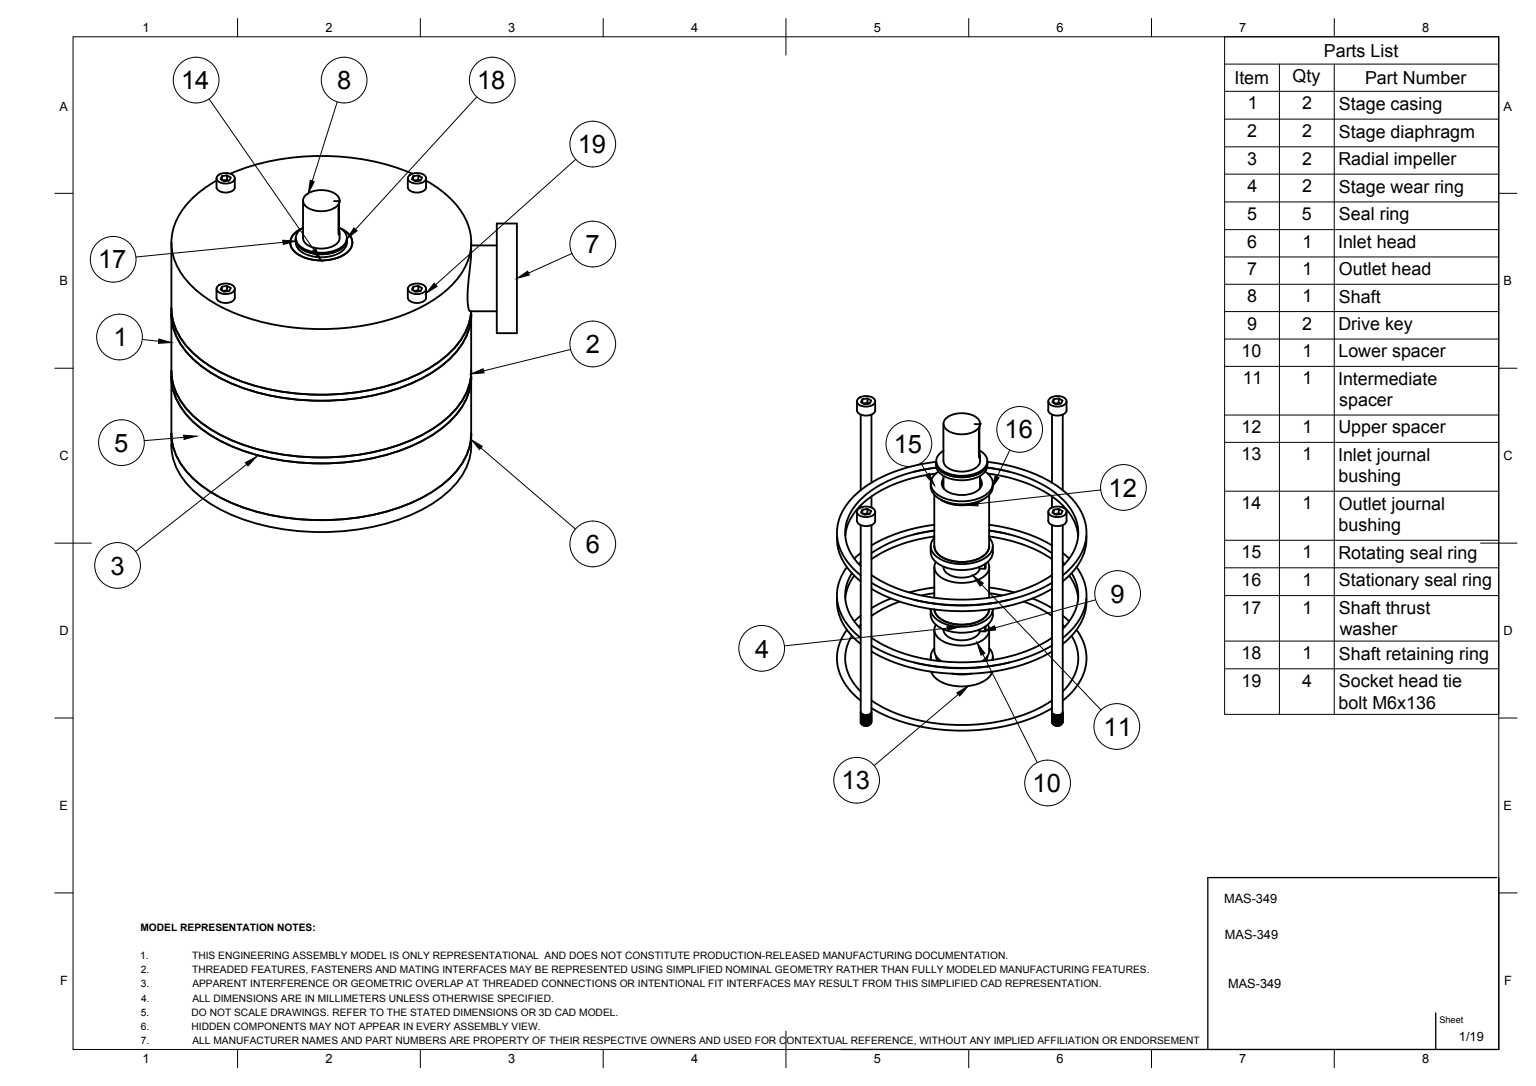
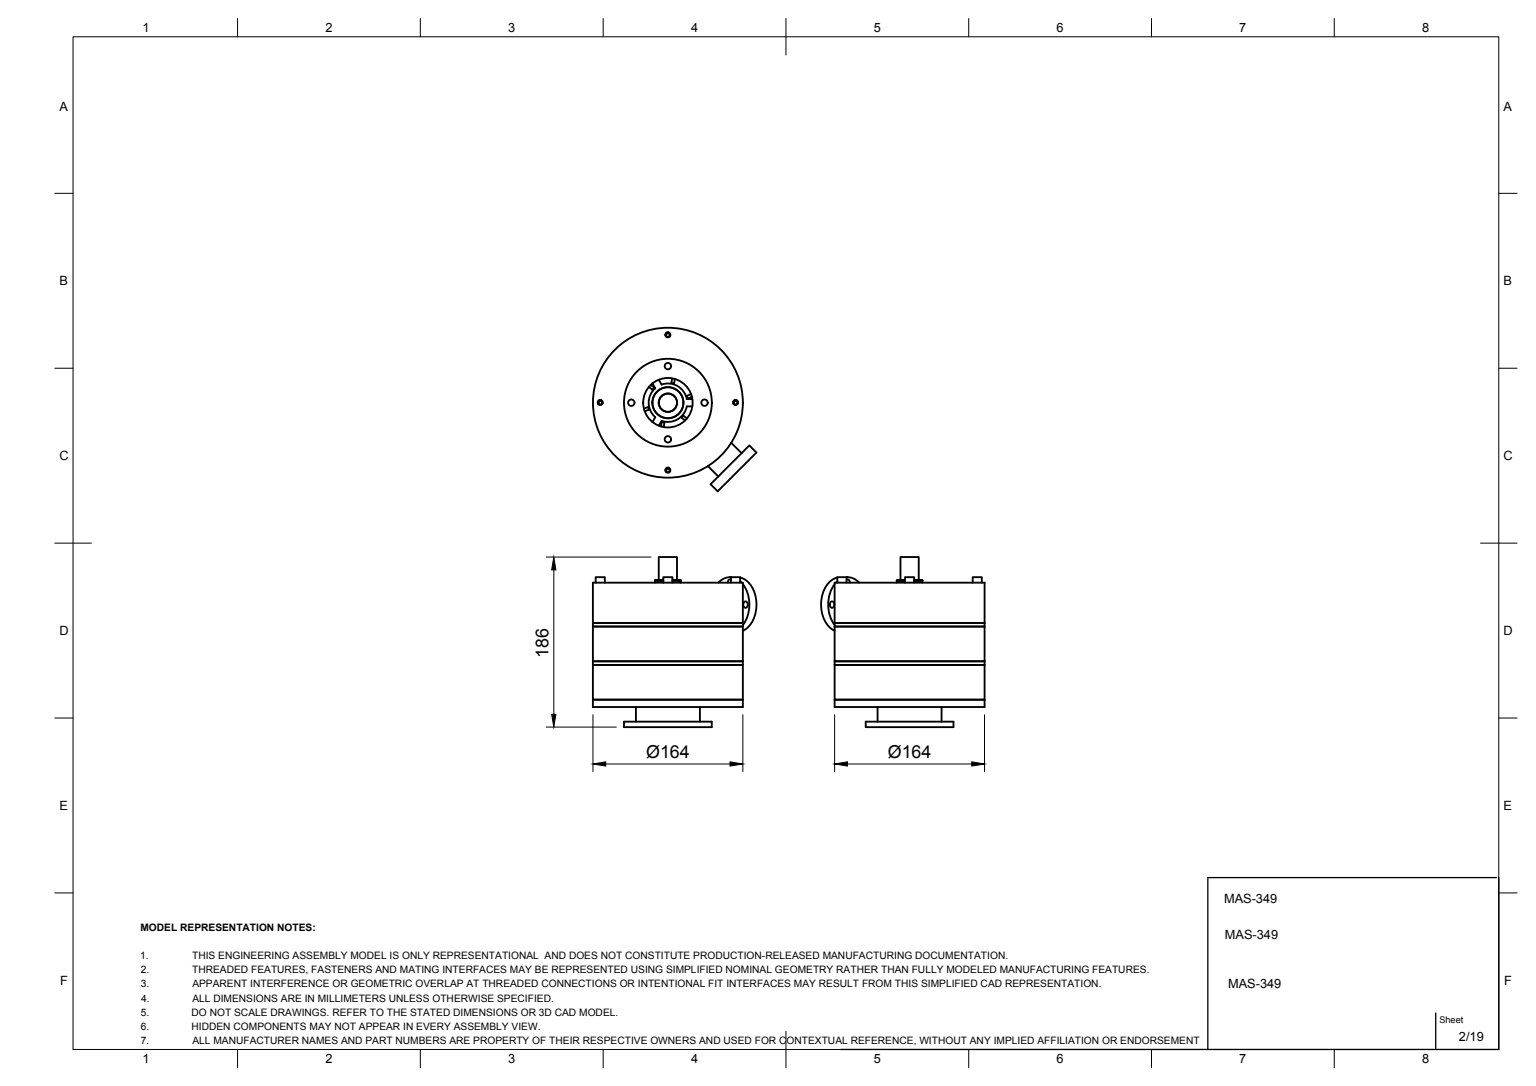
ISO-10303-21;
HEADER;
/* Generated by software containing ST-Developer
 * from STEP Tools, Inc. (www.steptools.com) 
 */

FILE_DESCRIPTION(
/* description */ ('Independent two-stage semi-open centrifugal-pump CAD. Shared impeller
s, open-machinable return casings, removable diaphragms, bronze wear/j
ournal rings, volume-preserving seal instances, retained keyed shaft, 
opposed mechanical face rings and partly threaded tie hardware. Native
 shaft rotation. Geometric topology/clearance only; flow/head/efficien
cy, pressure, cavitation, balance, preload, face loading and secondary
 seal fits/bonds, material/thermal/tolerance selection and life unassi
gned. External drive, coupling, anchors and piping bolts omitted.'),
/* implementation_level */ '2;1');

FILE_NAME(
/* name */ 'MAS-349.step',
/* time_stamp */ '2026-11-08T18:06:32-08:00',
/* author */ (''),
/* organization */ (''),
/* preprocessor_version */ 'ST-DEVELOPER v20.2',
/* originating_system */ 'Autodesk Translation Framework v15.17.0.0',
/* authorisation */ '');

FILE_SCHEMA (('AUTOMOTIVE_DESIGN { 1 0 10303 214 3 1 1 }'));
ENDSEC;

DATA;
#10=MECHANICAL_DESIGN_GEOMETRIC_PRESENTATION_REPRESENTATION('',(#393,#394,
#395,#396,#397,#398,#399,#400,#401,#402,#403,#404,#405,#406,#407,#408,#409,
#410,#411),#16687);
#11=ITEM_DEFINED_TRANSFORMATION($,$,#6342,#6957);
#12=ITEM_DEFINED_TRANSFORMATION($,$,#6451,#6958);
#13=ITEM_DEFINED_TRANSFORMATION($,$,#6480,#6959);
#14=ITEM_DEFINED_TRANSFORMATION($,$,#6553,#6960);
#15=ITEM_DEFINED_TRANSFORMATION($,$,#6342,#6961);
#16=ITEM_DEFINED_TRANSFORMATION($,$,#6451,#6962);
#17=ITEM_DEFINED_TRANSFORMATION($,$,#6480,#6963);
#18=ITEM_DEFINED_TRANSFORMATION($,$,#6712,#6964);
#19=ITEM_DEFINED_TRANSFORMATION($,$,#6553,#6965);
#20=ITEM_DEFINED_TRANSFORMATION($,$,#6562,#6966);
#21=ITEM_DEFINED_TRANSFORMATION($,$,#6712,#6967);
#22=ITEM_DEFINED_TRANSFORMATION($,$,#6712,#6968);
#23=ITEM_DEFINED_TRANSFORMATION($,$,#6712,#6969);
#24=ITEM_DEFINED_TRANSFORMATION($,$,#6712,#6970);
#25=ITEM_DEFINED_TRANSFORMATION($,$,#6715,#6971);
#26=ITEM_DEFINED_TRANSFORMATION($,$,#6778,#6972);
#27=ITEM_DEFINED_TRANSFORMATION($,$,#6860,#6973);
#28=ITEM_DEFINED_TRANSFORMATION($,$,#6824,#6974);
#29=ITEM_DEFINED_TRANSFORMATION($,$,#6833,#6975);
#30=ITEM_DEFINED_TRANSFORMATION($,$,#6842,#6976);
#31=ITEM_DEFINED_TRANSFORMATION($,$,#6851,#6977);
#32=ITEM_DEFINED_TRANSFORMATION($,$,#6860,#6978);
#33=ITEM_DEFINED_TRANSFORMATION($,$,#6871,#6979);
#34=ITEM_DEFINED_TRANSFORMATION($,$,#6880,#6980);
#35=ITEM_DEFINED_TRANSFORMATION($,$,#6889,#6981);
#36=ITEM_DEFINED_TRANSFORMATION($,$,#6898,#6982);
#37=ITEM_DEFINED_TRANSFORMATION($,$,#6907,#6983);
#38=ITEM_DEFINED_TRANSFORMATION($,$,#6918,#6984);
#39=ITEM_DEFINED_TRANSFORMATION($,$,#6918,#6985);
#40=ITEM_DEFINED_TRANSFORMATION($,$,#6918,#6986);
#41=ITEM_DEFINED_TRANSFORMATION($,$,#6918,#6987);
#42=(
REPRESENTATION_RELATIONSHIP($,$,#16764,#16763)
REPRESENTATION_RELATIONSHIP_WITH_TRANSFORMATION(#11)
SHAPE_REPRESENTATION_RELATIONSHIP()
);
#43=(
REPRESENTATION_RELATIONSHIP($,$,#16765,#16763)
REPRESENTATION_RELATIONSHIP_WITH_TRANSFORMATION(#12)
SHAPE_REPRESENTATION_RELATIONSHIP()
);
#44=(
REPRESENTATION_RELATIONSHIP($,$,#16766,#16763)
REPRESENTATION_RELATIONSHIP_WITH_TRANSFORMATION(#13)
SHAPE_REPRESENTATION_RELATIONSHIP()
);
#45=(
REPRESENTATION_RELATIONSHIP($,$,#16767,#16763)
REPRESENTATION_RELATIONSHIP_WITH_TRANSFORMATION(#14)
SHAPE_REPRESENTATION_RELATIONSHIP()
);
#46=(
REPRESENTATION_RELATIONSHIP($,$,#16764,#16763)
REPRESENTATION_RELATIONSHIP_WITH_TRANSFORMATION(#15)
SHAPE_REPRESENTATION_RELATIONSHIP()
);
#47=(
REPRESENTATION_RELATIONSHIP($,$,#16765,#16763)
REPRESENTATION_RELATIONSHIP_WITH_TRANSFORMATION(#16)
SHAPE_REPRESENTATION_RELATIONSHIP()
);
#48=(
REPRESENTATION_RELATIONSHIP($,$,#16766,#16763)
REPRESENTATION_RELATIONSHIP_WITH_TRANSFORMATION(#17)
SHAPE_REPRESENTATION_RELATIONSHIP()
);
#49=(
REPRESENTATION_RELATIONSHIP($,$,#16769,#16763)
REPRESENTATION_RELATIONSHIP_WITH_TRANSFORMATION(#18)
SHAPE_REPRESENTATION_RELATIONSHIP()
);
#50=(
REPRESENTATION_RELATIONSHIP($,$,#16767,#16763)
REPRESENTATION_RELATIONSHIP_WITH_TRANSFORMATION(#19)
SHAPE_REPRESENTATION_RELATIONSHIP()
);
#51=(
REPRESENTATION_RELATIONSHIP($,$,#16768,#16763)
REPRESENTATION_RELATIONSHIP_WITH_TRANSFORMATION(#20)
SHAPE_REPRESENTATION_RELATIONSHIP()
);
#52=(
REPRESENTATION_RELATIONSHIP($,$,#16769,#16763)
REPRESENTATION_RELATIONSHIP_WITH_TRANSFORMATION(#21)
SHAPE_REPRESENTATION_RELATIONSHIP()
);
#53=(
REPRESENTATION_RELATIONSHIP($,$,#16769,#16763)
REPRESENTATION_RELATIONSHIP_WITH_TRANSFORMATION(#22)
SHAPE_REPRESENTATION_RELATIONSHIP()
);
#54=(
REPRESENTATION_RELATIONSHIP($,$,#16769,#16763)
REPRESENTATION_RELATIONSHIP_WITH_TRANSFORMATION(#23)
SHAPE_REPRESENTATION_RELATIONSHIP()
);
#55=(
REPRESENTATION_RELATIONSHIP($,$,#16769,#16763)
REPRESENTATION_RELATIONSHIP_WITH_TRANSFORMATION(#24)
SHAPE_REPRESENTATION_RELATIONSHIP()
);
#56=(
REPRESENTATION_RELATIONSHIP($,$,#16770,#16763)
REPRESENTATION_RELATIONSHIP_WITH_TRANSFORMATION(#25)
SHAPE_REPRESENTATION_RELATIONSHIP()
);
#57=(
REPRESENTATION_RELATIONSHIP($,$,#16771,#16763)
REPRESENTATION_RELATIONSHIP_WITH_TRANSFORMATION(#26)
SHAPE_REPRESENTATION_RELATIONSHIP()
);
#58=(
REPRESENTATION_RELATIONSHIP($,$,#16776,#16763)
REPRESENTATION_RELATIONSHIP_WITH_TRANSFORMATION(#27)
SHAPE_REPRESENTATION_RELATIONSHIP()
);
#59=(
REPRESENTATION_RELATIONSHIP($,$,#16772,#16763)
REPRESENTATION_RELATIONSHIP_WITH_TRANSFORMATION(#28)
SHAPE_REPRESENTATION_RELATIONSHIP()
);
#60=(
REPRESENTATION_RELATIONSHIP($,$,#16773,#16763)
REPRESENTATION_RELATIONSHIP_WITH_TRANSFORMATION(#29)
SHAPE_REPRESENTATION_RELATIONSHIP()
);
#61=(
REPRESENTATION_RELATIONSHIP($,$,#16774,#16763)
REPRESENTATION_RELATIONSHIP_WITH_TRANSFORMATION(#30)
SHAPE_REPRESENTATION_RELATIONSHIP()
);
#62=(
REPRESENTATION_RELATIONSHIP($,$,#16775,#16763)
REPRESENTATION_RELATIONSHIP_WITH_TRANSFORMATION(#31)
SHAPE_REPRESENTATION_RELATIONSHIP()
);
#63=(
REPRESENTATION_RELATIONSHIP($,$,#16776,#16763)
REPRESENTATION_RELATIONSHIP_WITH_TRANSFORMATION(#32)
SHAPE_REPRESENTATION_RELATIONSHIP()
);
#64=(
REPRESENTATION_RELATIONSHIP($,$,#16777,#16763)
REPRESENTATION_RELATIONSHIP_WITH_TRANSFORMATION(#33)
SHAPE_REPRESENTATION_RELATIONSHIP()
);
#65=(
REPRESENTATION_RELATIONSHIP($,$,#16778,#16763)
REPRESENTATION_RELATIONSHIP_WITH_TRANSFORMATION(#34)
SHAPE_REPRESENTATION_RELATIONSHIP()
);
#66=(
REPRESENTATION_RELATIONSHIP($,$,#16779,#16763)
REPRESENTATION_RELATIONSHIP_WITH_TRANSFORMATION(#35)
SHAPE_REPRESENTATION_RELATIONSHIP()
);
#67=(
REPRESENTATION_RELATIONSHIP($,$,#16780,#16763)
REPRESENTATION_RELATIONSHIP_WITH_TRANSFORMATION(#36)
SHAPE_REPRESENTATION_RELATIONSHIP()
);
#68=(
REPRESENTATION_RELATIONSHIP($,$,#16781,#16763)
REPRESENTATION_RELATIONSHIP_WITH_TRANSFORMATION(#37)
SHAPE_REPRESENTATION_RELATIONSHIP()
);
#69=(
REPRESENTATION_RELATIONSHIP($,$,#16782,#16763)
REPRESENTATION_RELATIONSHIP_WITH_TRANSFORMATION(#38)
SHAPE_REPRESENTATION_RELATIONSHIP()
);
#70=(
REPRESENTATION_RELATIONSHIP($,$,#16782,#16763)
REPRESENTATION_RELATIONSHIP_WITH_TRANSFORMATION(#39)
SHAPE_REPRESENTATION_RELATIONSHIP()
);
#71=(
REPRESENTATION_RELATIONSHIP($,$,#16782,#16763)
REPRESENTATION_RELATIONSHIP_WITH_TRANSFORMATION(#40)
SHAPE_REPRESENTATION_RELATIONSHIP()
);
#72=(
REPRESENTATION_RELATIONSHIP($,$,#16782,#16763)
REPRESENTATION_RELATIONSHIP_WITH_TRANSFORMATION(#41)
SHAPE_REPRESENTATION_RELATIONSHIP()
);
#73=CONTEXT_DEPENDENT_SHAPE_REPRESENTATION(#42,#16732);
#74=CONTEXT_DEPENDENT_SHAPE_REPRESENTATION(#43,#16733);
#75=CONTEXT_DEPENDENT_SHAPE_REPRESENTATION(#44,#16734);
#76=CONTEXT_DEPENDENT_SHAPE_REPRESENTATION(#45,#16735);
#77=CONTEXT_DEPENDENT_SHAPE_REPRESENTATION(#46,#16736);
#78=CONTEXT_DEPENDENT_SHAPE_REPRESENTATION(#47,#16737);
#79=CONTEXT_DEPENDENT_SHAPE_REPRESENTATION(#48,#16738);
#80=CONTEXT_DEPENDENT_SHAPE_REPRESENTATION(#49,#16739);
#81=CONTEXT_DEPENDENT_SHAPE_REPRESENTATION(#50,#16740);
#82=CONTEXT_DEPENDENT_SHAPE_REPRESENTATION(#51,#16741);
#83=CONTEXT_DEPENDENT_SHAPE_REPRESENTATION(#52,#16742);
#84=CONTEXT_DEPENDENT_SHAPE_REPRESENTATION(#53,#16743);
#85=CONTEXT_DEPENDENT_SHAPE_REPRESENTATION(#54,#16744);
#86=CONTEXT_DEPENDENT_SHAPE_REPRESENTATION(#55,#16745);
#87=CONTEXT_DEPENDENT_SHAPE_REPRESENTATION(#56,#16746);
#88=CONTEXT_DEPENDENT_SHAPE_REPRESENTATION(#57,#16747);
#89=CONTEXT_DEPENDENT_SHAPE_REPRESENTATION(#58,#16748);
#90=CONTEXT_DEPENDENT_SHAPE_REPRESENTATION(#59,#16749);
#91=CONTEXT_DEPENDENT_SHAPE_REPRESENTATION(#60,#16750);
#92=CONTEXT_DEPENDENT_SHAPE_REPRESENTATION(#61,#16751);
#93=CONTEXT_DEPENDENT_SHAPE_REPRESENTATION(#62,#16752);
#94=CONTEXT_DEPENDENT_SHAPE_REPRESENTATION(#63,#16753);
#95=CONTEXT_DEPENDENT_SHAPE_REPRESENTATION(#64,#16754);
#96=CONTEXT_DEPENDENT_SHAPE_REPRESENTATION(#65,#16755);
#97=CONTEXT_DEPENDENT_SHAPE_REPRESENTATION(#66,#16756);
#98=CONTEXT_DEPENDENT_SHAPE_REPRESENTATION(#67,#16757);
#99=CONTEXT_DEPENDENT_SHAPE_REPRESENTATION(#68,#16758);
#100=CONTEXT_DEPENDENT_SHAPE_REPRESENTATION(#69,#16759);
#101=CONTEXT_DEPENDENT_SHAPE_REPRESENTATION(#70,#16760);
#102=CONTEXT_DEPENDENT_SHAPE_REPRESENTATION(#71,#16761);
#103=CONTEXT_DEPENDENT_SHAPE_REPRESENTATION(#72,#16762);
#104=NEXT_ASSEMBLY_USAGE_OCCURRENCE('Stage casing:1','Stage casing:1',
'Stage casing:1',#16784,#16785,'Stage casing:1');
#105=NEXT_ASSEMBLY_USAGE_OCCURRENCE('Stage diaphragm:1',
'Stage diaphragm:1','Stage diaphragm:1',#16784,#16786,
'Stage diaphragm:1');
#106=NEXT_ASSEMBLY_USAGE_OCCURRENCE('Radial impeller:1',
'Radial impeller:1','Radial impeller:1',#16784,#16787,
'Radial impeller:1');
#107=NEXT_ASSEMBLY_USAGE_OCCURRENCE('Stage wear ring:1',
'Stage wear ring:1','Stage wear ring:1',#16784,#16788,
'Stage wear ring:1');
#108=NEXT_ASSEMBLY_USAGE_OCCURRENCE('Stage casing:2','Stage casing:2',
'Stage casing:2',#16784,#16785,'Stage casing:2');
#109=NEXT_ASSEMBLY_USAGE_OCCURRENCE('Stage diaphragm:2',
'Stage diaphragm:2','Stage diaphragm:2',#16784,#16786,
'Stage diaphragm:2');
#110=NEXT_ASSEMBLY_USAGE_OCCURRENCE('Radial impeller:2',
'Radial impeller:2','Radial impeller:2',#16784,#16787,
'Radial impeller:2');
#111=NEXT_ASSEMBLY_USAGE_OCCURRENCE('Seal ring:1','Seal ring:1',
'Seal ring:1',#16784,#16790,'Seal ring:1');
#112=NEXT_ASSEMBLY_USAGE_OCCURRENCE('Stage wear ring:2',
'Stage wear ring:2','Stage wear ring:2',#16784,#16788,
'Stage wear ring:2');
#113=NEXT_ASSEMBLY_USAGE_OCCURRENCE('Inlet head:1','Inlet head:1',
'Inlet head:1',#16784,#16789,'Inlet head:1');
#114=NEXT_ASSEMBLY_USAGE_OCCURRENCE('Seal ring:2','Seal ring:2',
'Seal ring:2',#16784,#16790,'Seal ring:2');
#115=NEXT_ASSEMBLY_USAGE_OCCURRENCE('Seal ring:3','Seal ring:3',
'Seal ring:3',#16784,#16790,'Seal ring:3');
#116=NEXT_ASSEMBLY_USAGE_OCCURRENCE('Seal ring:4','Seal ring:4',
'Seal ring:4',#16784,#16790,'Seal ring:4');
#117=NEXT_ASSEMBLY_USAGE_OCCURRENCE('Seal ring:5','Seal ring:5',
'Seal ring:5',#16784,#16790,'Seal ring:5');
#118=NEXT_ASSEMBLY_USAGE_OCCURRENCE('Outlet head:1','Outlet head:1',
'Outlet head:1',#16784,#16791,'Outlet head:1');
#119=NEXT_ASSEMBLY_USAGE_OCCURRENCE('Shaft:1','Shaft:1','Shaft:1',#16784,
#16792,'Shaft:1');
#120=NEXT_ASSEMBLY_USAGE_OCCURRENCE('Drive key:1','Drive key:1',
'Drive key:1',#16784,#16797,'Drive key:1');
#121=NEXT_ASSEMBLY_USAGE_OCCURRENCE('Lower spacer:1','Lower spacer:1',
'Lower spacer:1',#16784,#16793,'Lower spacer:1');
#122=NEXT_ASSEMBLY_USAGE_OCCURRENCE('Intermediate spacer:1',
'Intermediate spacer:1','Intermediate spacer:1',#16784,#16794,
'Intermediate spacer:1');
#123=NEXT_ASSEMBLY_USAGE_OCCURRENCE('Upper spacer:1','Upper spacer:1',
'Upper spacer:1',#16784,#16795,'Upper spacer:1');
#124=NEXT_ASSEMBLY_USAGE_OCCURRENCE('Inlet journal bushing:1',
'Inlet journal bushing:1','Inlet journal bushing:1',#16784,#16796,
'Inlet journal bushing:1');
#125=NEXT_ASSEMBLY_USAGE_OCCURRENCE('Drive key:2','Drive key:2',
'Drive key:2',#16784,#16797,'Drive key:2');
#126=NEXT_ASSEMBLY_USAGE_OCCURRENCE('Outlet journal bushing:1',
'Outlet journal bushing:1','Outlet journal bushing:1',#16784,#16798,
'Outlet journal bushing:1');
#127=NEXT_ASSEMBLY_USAGE_OCCURRENCE('Rotating seal ring:1',
'Rotating seal ring:1','Rotating seal ring:1',#16784,#16799,
'Rotating seal ring:1');
#128=NEXT_ASSEMBLY_USAGE_OCCURRENCE('Stationary seal ring:1',
'Stationary seal ring:1','Stationary seal ring:1',#16784,#16800,
'Stationary seal ring:1');
#129=NEXT_ASSEMBLY_USAGE_OCCURRENCE('Shaft thrust washer:1',
'Shaft thrust washer:1','Shaft thrust washer:1',#16784,#16801,
'Shaft thrust washer:1');
#130=NEXT_ASSEMBLY_USAGE_OCCURRENCE('Shaft retaining ring:1',
'Shaft retaining ring:1','Shaft retaining ring:1',#16784,#16802,
'Shaft retaining ring:1');
#131=NEXT_ASSEMBLY_USAGE_OCCURRENCE('Socket head tie bolt M6x136:1',
'Socket head tie bolt M6x136:1','Socket head tie bolt M6x136:1',#16784,
#16803,'Socket head tie bolt M6x136:1');
#132=NEXT_ASSEMBLY_USAGE_OCCURRENCE('Socket head tie bolt M6x136:2',
'Socket head tie bolt M6x136:2','Socket head tie bolt M6x136:2',#16784,
#16803,'Socket head tie bolt M6x136:2');
#133=NEXT_ASSEMBLY_USAGE_OCCURRENCE('Socket head tie bolt M6x136:3',
'Socket head tie bolt M6x136:3','Socket head tie bolt M6x136:3',#16784,
#16803,'Socket head tie bolt M6x136:3');
#134=NEXT_ASSEMBLY_USAGE_OCCURRENCE('Socket head tie bolt M6x136:4',
'Socket head tie bolt M6x136:4','Socket head tie bolt M6x136:4',#16784,
#16803,'Socket head tie bolt M6x136:4');
#135=CONICAL_SURFACE('',#6937,0.25,0.78539816339745);
#136=ELLIPSE('',#6713,0.225,0.1);
#137=(
BOUNDED_SURFACE()
B_SPLINE_SURFACE(2,2,((#14548,#14549,#14550,#14551,#14552,#14553,#14554,
#14555,#14556),(#14557,#14558,#14559,#14560,#14561,#14562,#14563,#14564,
#14565),(#14566,#14567,#14568,#14569,#14570,#14571,#14572,#14573,#14574),
(#14575,#14576,#14577,#14578,#14579,#14580,#14581,#14582,#14583),(#14584,
#14585,#14586,#14587,#14588,#14589,#14590,#14591,#14592),(#14593,#14594,
#14595,#14596,#14597,#14598,#14599,#14600,#14601),(#14602,#14603,#14604,
#14605,#14606,#14607,#14608,#14609,#14610),(#14611,#14612,#14613,#14614,
#14615,#14616,#14617,#14618,#14619),(#14620,#14621,#14622,#14623,#14624,
#14625,#14626,#14627,#14628)),.UNSPECIFIED.,.T.,.T.,.F.)
B_SPLINE_SURFACE_WITH_KNOTS((3,2,2,2,3),(3,2,2,2,3),(-3.14159265358979,
-1.5707963267949,0.,1.5707963267949,3.14159265358979),(0.,1.5707963267949,
3.14159265358979,4.71238898038469,6.28318530717959),.UNSPECIFIED.)
GEOMETRIC_REPRESENTATION_ITEM()
RATIONAL_B_SPLINE_SURFACE(((1.,0.707106781186548,1.,0.707106781186548,1.,
0.707106781186548,1.,0.707106781186548,1.),(0.707106781186547,0.5,0.707106781186547,
0.5,0.707106781186547,0.5,0.707106781186547,0.5,0.707106781186547),(1.,
0.707106781186548,1.,0.707106781186548,1.,0.707106781186548,1.,0.707106781186548,
1.),(0.707106781186547,0.499999999999999,0.707106781186547,0.499999999999999,
0.707106781186547,0.499999999999999,0.707106781186547,0.499999999999999,
0.707106781186547),(1.,0.707106781186548,1.,0.707106781186548,1.,0.707106781186548,
1.,0.707106781186548,1.),(0.707106781186547,0.499999999999999,0.707106781186547,
0.499999999999999,0.707106781186547,0.499999999999999,0.707106781186547,
0.499999999999999,0.707106781186547),(1.,0.707106781186548,1.,0.707106781186548,
1.,0.707106781186548,1.,0.707106781186548,1.),(0.707106781186546,0.499999999999999,
0.707106781186546,0.499999999999999,0.707106781186546,0.499999999999999,
0.707106781186546,0.499999999999999,0.707106781186546),(1.,0.707106781186548,
1.,0.707106781186548,1.,0.707106781186548,1.,0.707106781186548,1.)))
REPRESENTATION_ITEM('')
SURFACE()
);
#138=B_SPLINE_SURFACE_WITH_KNOTS('',3,3,((#11457,#11458,#11459,#11460,#11461,
#11462,#11463,#11464,#11465,#11466,#11467,#11468,#11469,#11470,#11471,#11472,
#11473,#11474,#11475,#11476,#11477,#11478,#11479,#11480,#11481,#11482,#11483,
#11484,#11485,#11486,#11487,#11488,#11489,#11490,#11491,#11492,#11493,#11494,
#11495,#11496,#11497,#11498,#11499,#11500,#11501,#11502,#11503,#11504,#11505,
#11506,#11507,#11508,#11509,#11510,#11511,#11512),(#11513,#11514,#11515,
#11516,#11517,#11518,#11519,#11520,#11521,#11522,#11523,#11524,#11525,#11526,
#11527,#11528,#11529,#11530,#11531,#11532,#11533,#11534,#11535,#11536,#11537,
#11538,#11539,#11540,#11541,#11542,#11543,#11544,#11545,#11546,#11547,#11548,
#11549,#11550,#11551,#11552,#11553,#11554,#11555,#11556,#11557,#11558,#11559,
#11560,#11561,#11562,#11563,#11564,#11565,#11566,#11567,#11568),(#11569,
#11570,#11571,#11572,#11573,#11574,#11575,#11576,#11577,#11578,#11579,#11580,
#11581,#11582,#11583,#11584,#11585,#11586,#11587,#11588,#11589,#11590,#11591,
#11592,#11593,#11594,#11595,#11596,#11597,#11598,#11599,#11600,#11601,#11602,
#11603,#11604,#11605,#11606,#11607,#11608,#11609,#11610,#11611,#11612,#11613,
#11614,#11615,#11616,#11617,#11618,#11619,#11620,#11621,#11622,#11623,#11624),
(#11625,#11626,#11627,#11628,#11629,#11630,#11631,#11632,#11633,#11634,
#11635,#11636,#11637,#11638,#11639,#11640,#11641,#11642,#11643,#11644,#11645,
#11646,#11647,#11648,#11649,#11650,#11651,#11652,#11653,#11654,#11655,#11656,
#11657,#11658,#11659,#11660,#11661,#11662,#11663,#11664,#11665,#11666,#11667,
#11668,#11669,#11670,#11671,#11672,#11673,#11674,#11675,#11676,#11677,#11678,
#11679,#11680)),.UNSPECIFIED.,.F.,.F.,.F.,(4,4),(4,1,1,1,1,1,1,1,1,1,1,
1,1,1,1,1,1,1,1,1,1,1,1,1,1,1,1,1,1,1,1,1,1,1,1,1,1,1,1,1,1,1,1,1,1,1,1,
1,1,1,1,1,1,4),(0.,0.0642013499338864),(11.8589888623078,12.8454497557128,
13.8319106491178,14.8183715425228,15.8048324359278,16.7912933293328,17.7777542227378,
18.7642151161428,19.7506760095478,20.7371369029528,21.7235977963578,22.7100586897628,
23.6965195831678,24.6829804765729,25.6694413699779,26.6559022633829,27.6423631567879,
28.6288240501929,29.6152849435979,30.6017458370029,31.5882067304079,32.5746676238129,
33.5611285172179,34.5475894106229,35.5340503040279,36.5205111974329,37.5069720908379,
38.4934329842429,39.4798938776479,40.4663547710529,41.4528156644579,42.4392765578629,
43.4257374512679,44.4121983446729,45.3986592380779,46.3851201314829,47.3715810248879,
48.3580419182929,49.3445028116979,50.3309637051029,51.3174245985079,52.3038854919129,
53.2903463853179,54.2768072787229,55.2632681721279,56.2497290655329,57.2361899589379,
58.222650852343,59.209111745748,60.195572639153,61.182033532558,62.168494425963,
63.154955319368,64.141416212773),.UNSPECIFIED.);
#139=B_SPLINE_SURFACE_WITH_KNOTS('',3,3,((#11822,#11823,#11824,#11825,#11826,
#11827,#11828,#11829,#11830,#11831,#11832,#11833,#11834,#11835,#11836,#11837,
#11838,#11839,#11840,#11841,#11842,#11843,#11844,#11845,#11846,#11847,#11848,
#11849,#11850,#11851,#11852,#11853,#11854,#11855,#11856,#11857,#11858,#11859,
#11860,#11861,#11862,#11863,#11864,#11865,#11866,#11867,#11868,#11869,#11870,
#11871,#11872,#11873,#11874,#11875,#11876,#11877),(#11878,#11879,#11880,
#11881,#11882,#11883,#11884,#11885,#11886,#11887,#11888,#11889,#11890,#11891,
#11892,#11893,#11894,#11895,#11896,#11897,#11898,#11899,#11900,#11901,#11902,
#11903,#11904,#11905,#11906,#11907,#11908,#11909,#11910,#11911,#11912,#11913,
#11914,#11915,#11916,#11917,#11918,#11919,#11920,#11921,#11922,#11923,#11924,
#11925,#11926,#11927,#11928,#11929,#11930,#11931,#11932,#11933),(#11934,
#11935,#11936,#11937,#11938,#11939,#11940,#11941,#11942,#11943,#11944,#11945,
#11946,#11947,#11948,#11949,#11950,#11951,#11952,#11953,#11954,#11955,#11956,
#11957,#11958,#11959,#11960,#11961,#11962,#11963,#11964,#11965,#11966,#11967,
#11968,#11969,#11970,#11971,#11972,#11973,#11974,#11975,#11976,#11977,#11978,
#11979,#11980,#11981,#11982,#11983,#11984,#11985,#11986,#11987,#11988,#11989),
(#11990,#11991,#11992,#11993,#11994,#11995,#11996,#11997,#11998,#11999,
#12000,#12001,#12002,#12003,#12004,#12005,#12006,#12007,#12008,#12009,#12010,
#12011,#12012,#12013,#12014,#12015,#12016,#12017,#12018,#12019,#12020,#12021,
#12022,#12023,#12024,#12025,#12026,#12027,#12028,#12029,#12030,#12031,#12032,
#12033,#12034,#12035,#12036,#12037,#12038,#12039,#12040,#12041,#12042,#12043,
#12044,#12045)),.UNSPECIFIED.,.F.,.F.,.F.,(4,4),(4,1,1,1,1,1,1,1,1,1,1,
1,1,1,1,1,1,1,1,1,1,1,1,1,1,1,1,1,1,1,1,1,1,1,1,1,1,1,1,1,1,1,1,1,1,1,1,
1,1,1,1,1,1,4),(0.,0.0642013499338864),(14.3984001269718,15.3848610203768,
16.3713219137818,17.3577828071869,18.3442437005919,19.3307045939969,20.3171654874019,
21.3036263808069,22.2900872742119,23.2765481676169,24.2630090610219,25.2494699544269,
26.2359308478319,27.2223917412369,28.2088526346419,29.1953135280469,30.1817744214519,
31.1682353148569,32.1546962082619,33.1411571016669,34.1276179950719,35.1140788884769,
36.1005397818819,37.0870006752869,38.0734615686919,39.0599224620969,40.0463833555019,
41.0328442489069,42.0193051423119,43.0057660357169,43.9922269291219,44.9786878225269,
45.9651487159319,46.9516096093369,47.9380705027419,48.9245313961469,49.9109922895519,
50.8974531829569,51.8839140763619,52.8703749697669,53.856835863172,54.843296756577,
55.829757649982,56.816218543387,57.802679436792,58.789140330197,59.775601223602,
60.762062117007,61.748523010412,62.734983903817,63.721444797222,64.707905690627,
65.694366584032,66.680827477437),.UNSPECIFIED.);
#140=B_SPLINE_SURFACE_WITH_KNOTS('',3,3,((#12562,#12563,#12564,#12565,#12566,
#12567,#12568,#12569,#12570,#12571,#12572,#12573,#12574,#12575,#12576,#12577,
#12578,#12579,#12580,#12581,#12582,#12583,#12584,#12585,#12586,#12587,#12588,
#12589,#12590,#12591,#12592,#12593,#12594,#12595,#12596,#12597,#12598,#12599,
#12600,#12601,#12602,#12603,#12604,#12605,#12606,#12607,#12608,#12609,#12610,
#12611,#12612,#12613,#12614,#12615,#12616,#12617),(#12618,#12619,#12620,
#12621,#12622,#12623,#12624,#12625,#12626,#12627,#12628,#12629,#12630,#12631,
#12632,#12633,#12634,#12635,#12636,#12637,#12638,#12639,#12640,#12641,#12642,
#12643,#12644,#12645,#12646,#12647,#12648,#12649,#12650,#12651,#12652,#12653,
#12654,#12655,#12656,#12657,#12658,#12659,#12660,#12661,#12662,#12663,#12664,
#12665,#12666,#12667,#12668,#12669,#12670,#12671,#12672,#12673),(#12674,
#12675,#12676,#12677,#12678,#12679,#12680,#12681,#12682,#12683,#12684,#12685,
#12686,#12687,#12688,#12689,#12690,#12691,#12692,#12693,#12694,#12695,#12696,
#12697,#12698,#12699,#12700,#12701,#12702,#12703,#12704,#12705,#12706,#12707,
#12708,#12709,#12710,#12711,#12712,#12713,#12714,#12715,#12716,#12717,#12718,
#12719,#12720,#12721,#12722,#12723,#12724,#12725,#12726,#12727,#12728,#12729),
(#12730,#12731,#12732,#12733,#12734,#12735,#12736,#12737,#12738,#12739,
#12740,#12741,#12742,#12743,#12744,#12745,#12746,#12747,#12748,#12749,#12750,
#12751,#12752,#12753,#12754,#12755,#12756,#12757,#12758,#12759,#12760,#12761,
#12762,#12763,#12764,#12765,#12766,#12767,#12768,#12769,#12770,#12771,#12772,
#12773,#12774,#12775,#12776,#12777,#12778,#12779,#12780,#12781,#12782,#12783,
#12784,#12785)),.UNSPECIFIED.,.F.,.F.,.F.,(4,4),(4,1,1,1,1,1,1,1,1,1,1,
1,1,1,1,1,1,1,1,1,1,1,1,1,1,1,1,1,1,1,1,1,1,1,1,1,1,1,1,1,1,1,1,1,1,1,1,
1,1,1,1,1,1,4),(0.,0.0642013499338865),(11.8589888623078,12.8454497557128,
13.8319106491178,14.8183715425228,15.8048324359278,16.7912933293328,17.7777542227378,
18.7642151161428,19.7506760095478,20.7371369029528,21.7235977963578,22.7100586897628,
23.6965195831678,24.6829804765728,25.6694413699778,26.6559022633828,27.6423631567879,
28.6288240501929,29.6152849435979,30.6017458370029,31.5882067304079,32.5746676238129,
33.5611285172179,34.5475894106229,35.5340503040279,36.5205111974329,37.5069720908379,
38.4934329842429,39.4798938776479,40.4663547710529,41.4528156644579,42.4392765578629,
43.4257374512679,44.4121983446729,45.3986592380779,46.3851201314829,47.3715810248879,
48.3580419182929,49.3445028116979,50.3309637051029,51.3174245985079,52.3038854919129,
53.2903463853179,54.2768072787229,55.2632681721279,56.2497290655329,57.2361899589379,
58.2226508523429,59.2091117457479,60.1955726391529,61.1820335325579,62.1684944259629,
63.154955319368,64.141416212773),.UNSPECIFIED.);
#141=B_SPLINE_SURFACE_WITH_KNOTS('',3,3,((#12869,#12870,#12871,#12872,#12873,
#12874,#12875,#12876,#12877,#12878,#12879,#12880,#12881,#12882,#12883,#12884,
#12885,#12886,#12887,#12888,#12889,#12890,#12891,#12892,#12893,#12894,#12895,
#12896,#12897,#12898,#12899,#12900,#12901,#12902,#12903,#12904,#12905,#12906,
#12907,#12908,#12909,#12910,#12911,#12912,#12913,#12914,#12915,#12916,#12917,
#12918,#12919,#12920,#12921,#12922,#12923,#12924),(#12925,#12926,#12927,
#12928,#12929,#12930,#12931,#12932,#12933,#12934,#12935,#12936,#12937,#12938,
#12939,#12940,#12941,#12942,#12943,#12944,#12945,#12946,#12947,#12948,#12949,
#12950,#12951,#12952,#12953,#12954,#12955,#12956,#12957,#12958,#12959,#12960,
#12961,#12962,#12963,#12964,#12965,#12966,#12967,#12968,#12969,#12970,#12971,
#12972,#12973,#12974,#12975,#12976,#12977,#12978,#12979,#12980),(#12981,
#12982,#12983,#12984,#12985,#12986,#12987,#12988,#12989,#12990,#12991,#12992,
#12993,#12994,#12995,#12996,#12997,#12998,#12999,#13000,#13001,#13002,#13003,
#13004,#13005,#13006,#13007,#13008,#13009,#13010,#13011,#13012,#13013,#13014,
#13015,#13016,#13017,#13018,#13019,#13020,#13021,#13022,#13023,#13024,#13025,
#13026,#13027,#13028,#13029,#13030,#13031,#13032,#13033,#13034,#13035,#13036),
(#13037,#13038,#13039,#13040,#13041,#13042,#13043,#13044,#13045,#13046,
#13047,#13048,#13049,#13050,#13051,#13052,#13053,#13054,#13055,#13056,#13057,
#13058,#13059,#13060,#13061,#13062,#13063,#13064,#13065,#13066,#13067,#13068,
#13069,#13070,#13071,#13072,#13073,#13074,#13075,#13076,#13077,#13078,#13079,
#13080,#13081,#13082,#13083,#13084,#13085,#13086,#13087,#13088,#13089,#13090,
#13091,#13092)),.UNSPECIFIED.,.F.,.F.,.F.,(4,4),(4,1,1,1,1,1,1,1,1,1,1,
1,1,1,1,1,1,1,1,1,1,1,1,1,1,1,1,1,1,1,1,1,1,1,1,1,1,1,1,1,1,1,1,1,1,1,1,
1,1,1,1,1,1,4),(0.,0.0642013499338865),(14.3984001269718,15.3848610203768,
16.3713219137818,17.3577828071869,18.3442437005919,19.3307045939969,20.3171654874019,
21.3036263808069,22.2900872742119,23.2765481676169,24.2630090610219,25.2494699544269,
26.2359308478319,27.2223917412369,28.2088526346419,29.1953135280469,30.1817744214519,
31.1682353148569,32.1546962082619,33.1411571016669,34.1276179950719,35.1140788884769,
36.1005397818819,37.0870006752869,38.0734615686919,39.0599224620969,40.0463833555019,
41.0328442489069,42.0193051423119,43.0057660357169,43.9922269291219,44.9786878225269,
45.9651487159319,46.9516096093369,47.9380705027419,48.9245313961469,49.9109922895519,
50.8974531829569,51.8839140763619,52.8703749697669,53.8568358631719,54.8432967565769,
55.8297576499819,56.816218543387,57.802679436792,58.789140330197,59.775601223602,
60.762062117007,61.748523010412,62.734983903817,63.721444797222,64.707905690627,
65.694366584032,66.680827477437),.UNSPECIFIED.);
#142=B_SPLINE_SURFACE_WITH_KNOTS('',3,3,((#13198,#13199,#13200,#13201,#13202,
#13203,#13204,#13205,#13206,#13207,#13208,#13209,#13210,#13211,#13212,#13213,
#13214,#13215,#13216,#13217,#13218,#13219,#13220,#13221,#13222,#13223,#13224,
#13225,#13226,#13227,#13228,#13229,#13230,#13231,#13232,#13233,#13234,#13235,
#13236,#13237,#13238,#13239,#13240,#13241,#13242,#13243,#13244,#13245,#13246,
#13247,#13248,#13249,#13250,#13251,#13252,#13253),(#13254,#13255,#13256,
#13257,#13258,#13259,#13260,#13261,#13262,#13263,#13264,#13265,#13266,#13267,
#13268,#13269,#13270,#13271,#13272,#13273,#13274,#13275,#13276,#13277,#13278,
#13279,#13280,#13281,#13282,#13283,#13284,#13285,#13286,#13287,#13288,#13289,
#13290,#13291,#13292,#13293,#13294,#13295,#13296,#13297,#13298,#13299,#13300,
#13301,#13302,#13303,#13304,#13305,#13306,#13307,#13308,#13309),(#13310,
#13311,#13312,#13313,#13314,#13315,#13316,#13317,#13318,#13319,#13320,#13321,
#13322,#13323,#13324,#13325,#13326,#13327,#13328,#13329,#13330,#13331,#13332,
#13333,#13334,#13335,#13336,#13337,#13338,#13339,#13340,#13341,#13342,#13343,
#13344,#13345,#13346,#13347,#13348,#13349,#13350,#13351,#13352,#13353,#13354,
#13355,#13356,#13357,#13358,#13359,#13360,#13361,#13362,#13363,#13364,#13365),
(#13366,#13367,#13368,#13369,#13370,#13371,#13372,#13373,#13374,#13375,
#13376,#13377,#13378,#13379,#13380,#13381,#13382,#13383,#13384,#13385,#13386,
#13387,#13388,#13389,#13390,#13391,#13392,#13393,#13394,#13395,#13396,#13397,
#13398,#13399,#13400,#13401,#13402,#13403,#13404,#13405,#13406,#13407,#13408,
#13409,#13410,#13411,#13412,#13413,#13414,#13415,#13416,#13417,#13418,#13419,
#13420,#13421)),.UNSPECIFIED.,.F.,.F.,.F.,(4,4),(4,1,1,1,1,1,1,1,1,1,1,
1,1,1,1,1,1,1,1,1,1,1,1,1,1,1,1,1,1,1,1,1,1,1,1,1,1,1,1,1,1,1,1,1,1,1,1,
1,1,1,1,1,1,4),(0.,0.0642013499338865),(11.8589888623078,12.8454497557128,
13.8319106491178,14.8183715425228,15.8048324359278,16.7912933293328,17.7777542227378,
18.7642151161428,19.7506760095478,20.7371369029528,21.7235977963578,22.7100586897628,
23.6965195831678,24.6829804765728,25.6694413699778,26.6559022633828,27.6423631567879,
28.6288240501929,29.6152849435979,30.6017458370029,31.5882067304079,32.5746676238129,
33.5611285172179,34.5475894106229,35.5340503040279,36.5205111974329,37.5069720908379,
38.4934329842429,39.4798938776479,40.4663547710529,41.4528156644579,42.4392765578629,
43.4257374512679,44.4121983446729,45.3986592380779,46.3851201314829,47.3715810248879,
48.3580419182929,49.3445028116979,50.3309637051029,51.3174245985079,52.3038854919129,
53.2903463853179,54.2768072787229,55.2632681721279,56.2497290655329,57.2361899589379,
58.2226508523429,59.2091117457479,60.1955726391529,61.1820335325579,62.1684944259629,
63.154955319368,64.141416212773),.UNSPECIFIED.);
#143=B_SPLINE_SURFACE_WITH_KNOTS('',3,3,((#13505,#13506,#13507,#13508,#13509,
#13510,#13511,#13512,#13513,#13514,#13515,#13516,#13517,#13518,#13519,#13520,
#13521,#13522,#13523,#13524,#13525,#13526,#13527,#13528,#13529,#13530,#13531,
#13532,#13533,#13534,#13535,#13536,#13537,#13538,#13539,#13540,#13541,#13542,
#13543,#13544,#13545,#13546,#13547,#13548,#13549,#13550,#13551,#13552,#13553,
#13554,#13555,#13556,#13557,#13558,#13559,#13560),(#13561,#13562,#13563,
#13564,#13565,#13566,#13567,#13568,#13569,#13570,#13571,#13572,#13573,#13574,
#13575,#13576,#13577,#13578,#13579,#13580,#13581,#13582,#13583,#13584,#13585,
#13586,#13587,#13588,#13589,#13590,#13591,#13592,#13593,#13594,#13595,#13596,
#13597,#13598,#13599,#13600,#13601,#13602,#13603,#13604,#13605,#13606,#13607,
#13608,#13609,#13610,#13611,#13612,#13613,#13614,#13615,#13616),(#13617,
#13618,#13619,#13620,#13621,#13622,#13623,#13624,#13625,#13626,#13627,#13628,
#13629,#13630,#13631,#13632,#13633,#13634,#13635,#13636,#13637,#13638,#13639,
#13640,#13641,#13642,#13643,#13644,#13645,#13646,#13647,#13648,#13649,#13650,
#13651,#13652,#13653,#13654,#13655,#13656,#13657,#13658,#13659,#13660,#13661,
#13662,#13663,#13664,#13665,#13666,#13667,#13668,#13669,#13670,#13671,#13672),
(#13673,#13674,#13675,#13676,#13677,#13678,#13679,#13680,#13681,#13682,
#13683,#13684,#13685,#13686,#13687,#13688,#13689,#13690,#13691,#13692,#13693,
#13694,#13695,#13696,#13697,#13698,#13699,#13700,#13701,#13702,#13703,#13704,
#13705,#13706,#13707,#13708,#13709,#13710,#13711,#13712,#13713,#13714,#13715,
#13716,#13717,#13718,#13719,#13720,#13721,#13722,#13723,#13724,#13725,#13726,
#13727,#13728)),.UNSPECIFIED.,.F.,.F.,.F.,(4,4),(4,1,1,1,1,1,1,1,1,1,1,
1,1,1,1,1,1,1,1,1,1,1,1,1,1,1,1,1,1,1,1,1,1,1,1,1,1,1,1,1,1,1,1,1,1,1,1,
1,1,1,1,1,1,4),(0.,0.0642013499338865),(14.3984001269718,15.3848610203768,
16.3713219137818,17.3577828071869,18.3442437005919,19.3307045939969,20.3171654874019,
21.3036263808069,22.2900872742119,23.2765481676169,24.2630090610219,25.2494699544269,
26.2359308478319,27.2223917412369,28.2088526346419,29.1953135280469,30.1817744214519,
31.1682353148569,32.1546962082619,33.1411571016669,34.1276179950719,35.1140788884769,
36.1005397818819,37.0870006752869,38.0734615686919,39.0599224620969,40.0463833555019,
41.0328442489069,42.0193051423119,43.0057660357169,43.9922269291219,44.9786878225269,
45.9651487159319,46.9516096093369,47.9380705027419,48.9245313961469,49.9109922895519,
50.8974531829569,51.8839140763619,52.8703749697669,53.856835863172,54.843296756577,
55.829757649982,56.816218543387,57.802679436792,58.789140330197,59.775601223602,
60.762062117007,61.748523010412,62.734983903817,63.721444797222,64.707905690627,
65.694366584032,66.680827477437),.UNSPECIFIED.);
#144=B_SPLINE_SURFACE_WITH_KNOTS('',3,3,((#13834,#13835,#13836,#13837,#13838,
#13839,#13840,#13841,#13842,#13843,#13844,#13845,#13846,#13847,#13848,#13849,
#13850,#13851,#13852,#13853,#13854,#13855,#13856,#13857,#13858,#13859,#13860,
#13861,#13862,#13863,#13864,#13865,#13866,#13867,#13868,#13869,#13870,#13871,
#13872,#13873,#13874,#13875,#13876,#13877,#13878,#13879,#13880,#13881,#13882,
#13883,#13884,#13885,#13886,#13887,#13888,#13889),(#13890,#13891,#13892,
#13893,#13894,#13895,#13896,#13897,#13898,#13899,#13900,#13901,#13902,#13903,
#13904,#13905,#13906,#13907,#13908,#13909,#13910,#13911,#13912,#13913,#13914,
#13915,#13916,#13917,#13918,#13919,#13920,#13921,#13922,#13923,#13924,#13925,
#13926,#13927,#13928,#13929,#13930,#13931,#13932,#13933,#13934,#13935,#13936,
#13937,#13938,#13939,#13940,#13941,#13942,#13943,#13944,#13945),(#13946,
#13947,#13948,#13949,#13950,#13951,#13952,#13953,#13954,#13955,#13956,#13957,
#13958,#13959,#13960,#13961,#13962,#13963,#13964,#13965,#13966,#13967,#13968,
#13969,#13970,#13971,#13972,#13973,#13974,#13975,#13976,#13977,#13978,#13979,
#13980,#13981,#13982,#13983,#13984,#13985,#13986,#13987,#13988,#13989,#13990,
#13991,#13992,#13993,#13994,#13995,#13996,#13997,#13998,#13999,#14000,#14001),
(#14002,#14003,#14004,#14005,#14006,#14007,#14008,#14009,#14010,#14011,
#14012,#14013,#14014,#14015,#14016,#14017,#14018,#14019,#14020,#14021,#14022,
#14023,#14024,#14025,#14026,#14027,#14028,#14029,#14030,#14031,#14032,#14033,
#14034,#14035,#14036,#14037,#14038,#14039,#14040,#14041,#14042,#14043,#14044,
#14045,#14046,#14047,#14048,#14049,#14050,#14051,#14052,#14053,#14054,#14055,
#14056,#14057)),.UNSPECIFIED.,.F.,.F.,.F.,(4,4),(4,1,1,1,1,1,1,1,1,1,1,
1,1,1,1,1,1,1,1,1,1,1,1,1,1,1,1,1,1,1,1,1,1,1,1,1,1,1,1,1,1,1,1,1,1,1,1,
1,1,1,1,1,1,4),(0.,0.0642013499338864),(11.8589888623078,12.8454497557128,
13.8319106491178,14.8183715425228,15.8048324359278,16.7912933293328,17.7777542227378,
18.7642151161428,19.7506760095478,20.7371369029528,21.7235977963578,22.7100586897628,
23.6965195831678,24.6829804765729,25.6694413699779,26.6559022633829,27.6423631567879,
28.6288240501929,29.6152849435979,30.6017458370029,31.5882067304079,32.5746676238129,
33.5611285172179,34.5475894106229,35.5340503040279,36.5205111974329,37.5069720908379,
38.4934329842429,39.4798938776479,40.4663547710529,41.4528156644579,42.4392765578629,
43.4257374512679,44.4121983446729,45.3986592380779,46.3851201314829,47.3715810248879,
48.3580419182929,49.3445028116979,50.3309637051029,51.3174245985079,52.3038854919129,
53.2903463853179,54.2768072787229,55.2632681721279,56.2497290655329,57.2361899589379,
58.222650852343,59.209111745748,60.195572639153,61.182033532558,62.168494425963,
63.154955319368,64.141416212773),.UNSPECIFIED.);
#145=B_SPLINE_SURFACE_WITH_KNOTS('',3,3,((#14141,#14142,#14143,#14144,#14145,
#14146,#14147,#14148,#14149,#14150,#14151,#14152,#14153,#14154,#14155,#14156,
#14157,#14158,#14159,#14160,#14161,#14162,#14163,#14164,#14165,#14166,#14167,
#14168,#14169,#14170,#14171,#14172,#14173,#14174,#14175,#14176,#14177,#14178,
#14179,#14180,#14181,#14182,#14183,#14184,#14185,#14186,#14187,#14188,#14189,
#14190,#14191,#14192,#14193,#14194,#14195,#14196),(#14197,#14198,#14199,
#14200,#14201,#14202,#14203,#14204,#14205,#14206,#14207,#14208,#14209,#14210,
#14211,#14212,#14213,#14214,#14215,#14216,#14217,#14218,#14219,#14220,#14221,
#14222,#14223,#14224,#14225,#14226,#14227,#14228,#14229,#14230,#14231,#14232,
#14233,#14234,#14235,#14236,#14237,#14238,#14239,#14240,#14241,#14242,#14243,
#14244,#14245,#14246,#14247,#14248,#14249,#14250,#14251,#14252),(#14253,
#14254,#14255,#14256,#14257,#14258,#14259,#14260,#14261,#14262,#14263,#14264,
#14265,#14266,#14267,#14268,#14269,#14270,#14271,#14272,#14273,#14274,#14275,
#14276,#14277,#14278,#14279,#14280,#14281,#14282,#14283,#14284,#14285,#14286,
#14287,#14288,#14289,#14290,#14291,#14292,#14293,#14294,#14295,#14296,#14297,
#14298,#14299,#14300,#14301,#14302,#14303,#14304,#14305,#14306,#14307,#14308),
(#14309,#14310,#14311,#14312,#14313,#14314,#14315,#14316,#14317,#14318,
#14319,#14320,#14321,#14322,#14323,#14324,#14325,#14326,#14327,#14328,#14329,
#14330,#14331,#14332,#14333,#14334,#14335,#14336,#14337,#14338,#14339,#14340,
#14341,#14342,#14343,#14344,#14345,#14346,#14347,#14348,#14349,#14350,#14351,
#14352,#14353,#14354,#14355,#14356,#14357,#14358,#14359,#14360,#14361,#14362,
#14363,#14364)),.UNSPECIFIED.,.F.,.F.,.F.,(4,4),(4,1,1,1,1,1,1,1,1,1,1,
1,1,1,1,1,1,1,1,1,1,1,1,1,1,1,1,1,1,1,1,1,1,1,1,1,1,1,1,1,1,1,1,1,1,1,1,
1,1,1,1,1,1,4),(0.,0.0642013499338864),(14.3984001269718,15.3848610203768,
16.3713219137818,17.3577828071869,18.3442437005919,19.3307045939969,20.3171654874019,
21.3036263808069,22.2900872742119,23.2765481676169,24.2630090610219,25.2494699544269,
26.2359308478319,27.2223917412369,28.2088526346419,29.1953135280469,30.1817744214519,
31.1682353148569,32.1546962082619,33.1411571016669,34.1276179950719,35.1140788884769,
36.1005397818819,37.0870006752869,38.0734615686919,39.0599224620969,40.0463833555019,
41.0328442489069,42.0193051423119,43.0057660357169,43.9922269291219,44.9786878225269,
45.9651487159319,46.9516096093369,47.9380705027419,48.9245313961469,49.9109922895519,
50.8974531829569,51.8839140763619,52.8703749697669,53.856835863172,54.843296756577,
55.829757649982,56.816218543387,57.802679436792,58.789140330197,59.775601223602,
60.762062117007,61.748523010412,62.734983903817,63.721444797222,64.707905690627,
65.694366584032,66.680827477437),.UNSPECIFIED.);
#146=B_SPLINE_SURFACE_WITH_KNOTS('',3,3,((#15976,#15977,#15978,#15979,#15980,
#15981,#15982,#15983,#15984,#15985,#15986,#15987,#15988,#15989,#15990,#15991,
#15992,#15993,#15994,#15995,#15996,#15997,#15998,#15999,#16000,#16001,#16002,
#16003,#16004,#16005,#16006,#16007,#16008,#16009,#16010,#16011,#16012,#16013,
#16014,#16015,#16016,#16017,#16018,#16019,#16020,#16021,#16022,#16023,#16024,
#16025,#16026),(#16027,#16028,#16029,#16030,#16031,#16032,#16033,#16034,
#16035,#16036,#16037,#16038,#16039,#16040,#16041,#16042,#16043,#16044,#16045,
#16046,#16047,#16048,#16049,#16050,#16051,#16052,#16053,#16054,#16055,#16056,
#16057,#16058,#16059,#16060,#16061,#16062,#16063,#16064,#16065,#16066,#16067,
#16068,#16069,#16070,#16071,#16072,#16073,#16074,#16075,#16076,#16077),
(#16078,#16079,#16080,#16081,#16082,#16083,#16084,#16085,#16086,#16087,
#16088,#16089,#16090,#16091,#16092,#16093,#16094,#16095,#16096,#16097,#16098,
#16099,#16100,#16101,#16102,#16103,#16104,#16105,#16106,#16107,#16108,#16109,
#16110,#16111,#16112,#16113,#16114,#16115,#16116,#16117,#16118,#16119,#16120,
#16121,#16122,#16123,#16124,#16125,#16126,#16127,#16128),(#16129,#16130,
#16131,#16132,#16133,#16134,#16135,#16136,#16137,#16138,#16139,#16140,#16141,
#16142,#16143,#16144,#16145,#16146,#16147,#16148,#16149,#16150,#16151,#16152,
#16153,#16154,#16155,#16156,#16157,#16158,#16159,#16160,#16161,#16162,#16163,
#16164,#16165,#16166,#16167,#16168,#16169,#16170,#16171,#16172,#16173,#16174,
#16175,#16176,#16177,#16178,#16179)),.UNSPECIFIED.,.F.,.F.,.F.,(4,4),(4,
1,1,1,1,1,1,1,1,1,1,1,1,1,1,1,1,1,1,1,1,1,1,1,1,1,1,1,1,1,1,1,1,1,1,1,1,
1,1,1,1,1,1,1,1,1,1,1,4),(0.,0.0658467982010765),(11.6150328478183,12.6135684378078,
13.6121040277972,14.6106396177866,15.609175207776,16.6077107977655,17.6062463877549,
18.6047819777443,19.6033175677338,20.6018531577232,21.6003887477126,22.5989243377021,
23.5974599276915,24.5959955176809,25.5945311076704,26.5930666976598,27.5916022876492,
28.5901378776387,29.5886734676281,30.5872090576175,31.585744647607,32.5842802375964,
33.5828158275858,34.5813514175752,35.5798870075647,36.5784225975541,37.5769581875435,
38.575493777533,39.5740293675224,40.5725649575118,41.5711005475013,42.5696361374907,
43.5681717274801,44.5667073174696,45.565242907459,46.5637784974484,47.5623140874379,
48.5608496774273,49.5593852674167,50.5579208574061,51.5564564473956,52.554992037385,
53.5535276273744,54.5520632173639,55.5505988073533,56.5491343973427,57.5476699873322,
58.5462055773216,59.544741167311),.UNSPECIFIED.);
#147=B_SPLINE_SURFACE_WITH_KNOTS('',3,3,((#16278,#16279,#16280,#16281,#16282,
#16283,#16284,#16285,#16286,#16287,#16288,#16289,#16290,#16291,#16292,#16293,
#16294,#16295,#16296,#16297,#16298,#16299,#16300,#16301,#16302,#16303,#16304,
#16305,#16306,#16307,#16308,#16309,#16310,#16311,#16312,#16313,#16314,#16315,
#16316,#16317,#16318,#16319,#16320,#16321,#16322,#16323,#16324,#16325,#16326,
#16327,#16328,#16329,#16330),(#16331,#16332,#16333,#16334,#16335,#16336,
#16337,#16338,#16339,#16340,#16341,#16342,#16343,#16344,#16345,#16346,#16347,
#16348,#16349,#16350,#16351,#16352,#16353,#16354,#16355,#16356,#16357,#16358,
#16359,#16360,#16361,#16362,#16363,#16364,#16365,#16366,#16367,#16368,#16369,
#16370,#16371,#16372,#16373,#16374,#16375,#16376,#16377,#16378,#16379,#16380,
#16381,#16382,#16383),(#16384,#16385,#16386,#16387,#16388,#16389,#16390,
#16391,#16392,#16393,#16394,#16395,#16396,#16397,#16398,#16399,#16400,#16401,
#16402,#16403,#16404,#16405,#16406,#16407,#16408,#16409,#16410,#16411,#16412,
#16413,#16414,#16415,#16416,#16417,#16418,#16419,#16420,#16421,#16422,#16423,
#16424,#16425,#16426,#16427,#16428,#16429,#16430,#16431,#16432,#16433,#16434,
#16435,#16436),(#16437,#16438,#16439,#16440,#16441,#16442,#16443,#16444,
#16445,#16446,#16447,#16448,#16449,#16450,#16451,#16452,#16453,#16454,#16455,
#16456,#16457,#16458,#16459,#16460,#16461,#16462,#16463,#16464,#16465,#16466,
#16467,#16468,#16469,#16470,#16471,#16472,#16473,#16474,#16475,#16476,#16477,
#16478,#16479,#16480,#16481,#16482,#16483,#16484,#16485,#16486,#16487,#16488,
#16489)),.UNSPECIFIED.,.F.,.F.,.F.,(4,4),(4,1,1,1,1,1,1,1,1,1,1,1,1,1,1,
1,1,1,1,1,1,1,1,1,1,1,1,1,1,1,1,1,1,1,1,1,1,1,1,1,1,1,1,1,1,1,1,1,1,1,4),
(0.,0.0658467982010765),(8.307477552401,9.30744448228904,10.3074114121771,
11.3073783420651,12.3073452719531,13.3073122018412,14.3072791317292,15.3072460616173,
16.3072129915053,17.3071799213933,18.3071468512814,19.3071137811694,20.3070807110574,
21.3070476409455,22.3070145708335,23.3069815007215,24.3069484306096,25.3069153604976,
26.3068822903856,27.3068492202737,28.3068161501617,29.3067830800498,30.3067500099378,
31.3067169398258,32.3066838697139,33.3066507996019,34.3066177294899,35.306584659378,
36.306551589266,37.306518519154,38.3064854490421,39.3064523789301,40.3064193088181,
41.3063862387062,42.3063531685942,43.3063200984823,44.3062870283703,45.3062539582583,
46.3062208881464,47.3061878180344,48.3061547479224,49.3061216778105,50.3060886076985,
51.3060555375865,52.3060224674746,53.3059893973626,54.3059563272507,55.3059232571387,
56.3058901870267,57.3058571169148,58.3058240468028),.UNSPECIFIED.);
#148=B_SPLINE_CURVE_WITH_KNOTS('',3,(#9202,#9203,#9204,#9205),
 .UNSPECIFIED.,.F.,.F.,(4,4),(51.5750455984138,52.2824273504652),
 .UNSPECIFIED.);
#149=B_SPLINE_CURVE_WITH_KNOTS('',3,(#9208,#9209,#9210,#9211,#9212,#9213,
#9214,#9215,#9216,#9217),.UNSPECIFIED.,.F.,.F.,(4,3,3,4),(-50.2654824574367,
-49.3230446702501,-48.3365837768451,-47.8312715558983),.UNSPECIFIED.);
#150=B_SPLINE_CURVE_WITH_KNOTS('',3,(#9222,#9223,#9224,#9225,#9226,#9227,
#9228,#9229,#9230,#9231,#9232,#9233,#9234,#9235,#9236,#9237,#9238,#9239,
#9240,#9241,#9242,#9243,#9244,#9245,#9246),.UNSPECIFIED.,.F.,.F.,(4,3,3,
3,3,3,3,3,4),(45.2918602912342,45.3772010966301,46.3636619900351,47.3501228834401,
48.3365837768451,49.3230446702501,50.3095055636551,51.2959664570601,51.5750455984138),
 .UNSPECIFIED.);
#151=B_SPLINE_CURVE_WITH_KNOTS('',3,(#9247,#9248,#9249,#9250,#9251,#9252,
#9253,#9254,#9255,#9256,#9257,#9258,#9259,#9260,#9261,#9262,#9263,#9264,
#9265,#9266,#9267,#9268),.UNSPECIFIED.,.F.,.F.,(4,3,3,3,3,3,3,4),(-47.8312715558983,
-47.3501228834401,-46.3636619900351,-45.3772010966301,-44.3907402032251,
-43.4042793098201,-42.4178184164151,-41.5480862487187),.UNSPECIFIED.);
#152=B_SPLINE_CURVE_WITH_KNOTS('',3,(#9273,#9274,#9275,#9276,#9277,#9278,
#9279,#9280,#9281,#9282,#9283,#9284,#9285,#9286,#9287,#9288,#9289,#9290,
#9291,#9292,#9293,#9294),.UNSPECIFIED.,.F.,.F.,(4,3,3,3,3,3,3,4),(39.0086749840546,
39.4584357362001,40.4448966296051,41.4313575230101,42.4178184164151,43.4042793098201,
44.3907402032251,45.2918602912342),.UNSPECIFIED.);
#153=B_SPLINE_CURVE_WITH_KNOTS('',3,(#9295,#9296,#9297,#9298,#9299,#9300,
#9301,#9302,#9303,#9304,#9305,#9306,#9307,#9308,#9309,#9310,#9311,#9312,
#9313,#9314,#9315,#9316,#9317,#9318,#9319),.UNSPECIFIED.,.F.,.F.,(4,3,3,
3,3,3,3,3,4),(-41.5480862487187,-41.4313575230101,-40.4448966296051,-39.4584357362001,
-38.4719748427951,-37.4855139493901,-36.4990530559851,-35.5125921625801,
-35.2649009415391),.UNSPECIFIED.);
#154=B_SPLINE_CURVE_WITH_KNOTS('',3,(#9324,#9325,#9326,#9327,#9328,#9329,
#9330,#9331,#9332,#9333,#9334,#9335,#9336,#9337,#9338,#9339,#9340,#9341,
#9342,#9343,#9344,#9345),.UNSPECIFIED.,.F.,.F.,(4,3,3,3,3,3,3,4),(32.725489676875,
33.5396703757701,34.5261312691751,35.5125921625801,36.4990530559851,37.4855139493901,
38.4719748427951,39.0086749840546),.UNSPECIFIED.);
#155=B_SPLINE_CURVE_WITH_KNOTS('',3,(#9346,#9347,#9348,#9349,#9350,#9351,
#9352,#9353,#9354,#9355,#9356,#9357,#9358,#9359,#9360,#9361,#9362,#9363,
#9364,#9365,#9366,#9367),.UNSPECIFIED.,.F.,.F.,(4,3,3,3,3,3,3,4),(-35.2649009415391,
-34.5261312691751,-33.5396703757701,-32.5532094823651,-31.5667485889601,
-30.5802876955551,-29.5938268021501,-28.9817156343595),.UNSPECIFIED.);
#156=B_SPLINE_CURVE_WITH_KNOTS('',3,(#9372,#9373,#9374,#9375,#9376,#9377,
#9378,#9379,#9380,#9381,#9382,#9383,#9384,#9385,#9386,#9387,#9388,#9389,
#9390,#9391,#9392,#9393,#9394,#9395,#9396),.UNSPECIFIED.,.F.,.F.,(4,3,3,
3,3,3,3,3,4),(26.4423043696954,26.6344441219351,27.6209050153401,28.6073659087451,
29.5938268021501,30.5802876955551,31.5667485889601,32.5532094823651,32.725489676875),
 .UNSPECIFIED.);
#157=B_SPLINE_CURVE_WITH_KNOTS('',3,(#9397,#9398,#9399,#9400,#9401,#9402,
#9403,#9404,#9405,#9406,#9407,#9408,#9409,#9410,#9411,#9412,#9413,#9414,
#9415,#9416,#9417,#9418),.UNSPECIFIED.,.F.,.F.,(4,3,3,3,3,3,3,4),(-28.9817156343595,
-28.6073659087451,-27.6209050153401,-26.6344441219351,-25.6479832285301,
-24.6615223351251,-23.6750614417201,-22.6985303271799),.UNSPECIFIED.);
#158=B_SPLINE_CURVE_WITH_KNOTS('',3,(#9423,#9424,#9425,#9426,#9427,#9428,
#9429,#9430,#9431,#9432,#9433,#9434,#9435,#9436,#9437,#9438,#9439,#9440,
#9441,#9442,#9443,#9444),.UNSPECIFIED.,.F.,.F.,(4,3,3,3,3,3,3,4),(20.1591190625159,
20.7156787615051,21.7021396549101,22.6886005483151,23.6750614417201,24.6615223351251,
25.6479832285301,26.4423043696954),.UNSPECIFIED.);
#159=B_SPLINE_CURVE_WITH_KNOTS('',3,(#9445,#9446,#9447,#9448,#9449,#9450,
#9451,#9452,#9453,#9454,#9455,#9456,#9457,#9458,#9459,#9460,#9461,#9462,
#9463,#9464,#9465,#9466,#9467,#9468,#9469),.UNSPECIFIED.,.F.,.F.,(4,3,3,
3,3,3,3,3,4),(-22.6985303271799,-22.6886005483151,-21.7021396549101,-20.7156787615051,
-19.7292178681001,-18.7427569746951,-17.75629608129,-16.7698351878851,-16.4153450200003),
 .UNSPECIFIED.);
#160=B_SPLINE_CURVE_WITH_KNOTS('',3,(#9474,#9475,#9476,#9477,#9478,#9479,
#9480,#9481,#9482,#9483,#9484,#9485,#9486,#9487,#9488,#9489,#9490,#9491,
#9492,#9493,#9494,#9495),.UNSPECIFIED.,.F.,.F.,(4,3,3,3,3,3,3,4),(13.8759337553363,
14.796913401075,15.78337429448,16.769835187885,17.75629608129,18.7427569746951,
19.7292178681001,20.1591190625159),.UNSPECIFIED.);
#161=B_SPLINE_CURVE_WITH_KNOTS('',3,(#9496,#9497,#9498,#9499,#9500,#9501,
#9502,#9503,#9504,#9505,#9506,#9507,#9508,#9509,#9510,#9511,#9512,#9513,
#9514,#9515,#9516,#9517),.UNSPECIFIED.,.F.,.F.,(4,3,3,3,3,3,3,4),(-16.4153450200003,
-15.78337429448,-14.796913401075,-13.81045250767,-12.823991614265,-11.83753072086,
-10.851069827455,-10.1321597128207),.UNSPECIFIED.);
#162=B_SPLINE_CURVE_WITH_KNOTS('',3,(#9523,#9524,#9525,#9526,#9527,#9528,
#9529,#9530,#9531,#9532,#9533,#9534,#9535),.UNSPECIFIED.,.F.,.F.,(4,3,3,
3,4),(-3.84897440564114,-2.95938268021501,-1.97292178681,-0.986460893405002,
0.),.UNSPECIFIED.);
#163=B_SPLINE_CURVE_WITH_KNOTS('',3,(#9538,#9539,#9540,#9541,#9542,#9543,
#9544,#9545,#9546,#9547,#9548,#9549,#9550,#9551,#9552,#9553,#9554,#9555,
#9556),.UNSPECIFIED.,.F.,.F.,(4,3,3,3,3,3,4),(2.01694489302845,2.95938268021501,
3.94584357362001,4.93230446702502,5.91876536043002,6.90522625383502,7.59274844815668),
 .UNSPECIFIED.);
#164=B_SPLINE_CURVE_WITH_KNOTS('',3,(#9562,#9563,#9564,#9565),
 .UNSPECIFIED.,.F.,.F.,(4,4),(51.5750455984138,52.2824273504652),
 .UNSPECIFIED.);
#165=B_SPLINE_CURVE_WITH_KNOTS('',3,(#9568,#9569,#9570,#9571,#9572,#9573,
#9574,#9575,#9576,#9577),.UNSPECIFIED.,.F.,.F.,(4,3,3,4),(-50.2654824574367,
-49.3230446702501,-48.3365837768451,-47.8312715558982),.UNSPECIFIED.);
#166=B_SPLINE_CURVE_WITH_KNOTS('',3,(#9582,#9583,#9584,#9585,#9586,#9587,
#9588,#9589,#9590,#9591,#9592,#9593,#9594,#9595,#9596,#9597,#9598,#9599,
#9600,#9601,#9602,#9603,#9604,#9605,#9606),.UNSPECIFIED.,.F.,.F.,(4,3,3,
3,3,3,3,3,4),(45.2918602912342,45.3772010966301,46.3636619900351,47.3501228834401,
48.3365837768451,49.3230446702501,50.3095055636551,51.2959664570602,51.5750455984138),
 .UNSPECIFIED.);
#167=B_SPLINE_CURVE_WITH_KNOTS('',3,(#9607,#9608,#9609,#9610,#9611,#9612,
#9613,#9614,#9615,#9616,#9617,#9618,#9619,#9620,#9621,#9622,#9623,#9624,
#9625,#9626,#9627,#9628),.UNSPECIFIED.,.F.,.F.,(4,3,3,3,3,3,3,4),(-47.8312715558982,
-47.3501228834401,-46.3636619900351,-45.3772010966301,-44.3907402032251,
-43.4042793098201,-42.4178184164151,-41.5480862487187),.UNSPECIFIED.);
#168=B_SPLINE_CURVE_WITH_KNOTS('',3,(#9633,#9634,#9635,#9636,#9637,#9638,
#9639,#9640,#9641,#9642,#9643,#9644,#9645,#9646,#9647,#9648,#9649,#9650,
#9651,#9652,#9653,#9654),.UNSPECIFIED.,.F.,.F.,(4,3,3,3,3,3,3,4),(39.0086749840546,
39.4584357362001,40.4448966296051,41.4313575230101,42.4178184164151,43.4042793098201,
44.3907402032251,45.2918602912342),.UNSPECIFIED.);
#169=B_SPLINE_CURVE_WITH_KNOTS('',3,(#9655,#9656,#9657,#9658,#9659,#9660,
#9661,#9662,#9663,#9664,#9665,#9666,#9667,#9668,#9669,#9670,#9671,#9672,
#9673,#9674,#9675,#9676,#9677,#9678,#9679),.UNSPECIFIED.,.F.,.F.,(4,3,3,
3,3,3,3,3,4),(-41.5480862487187,-41.4313575230101,-40.4448966296051,-39.4584357362001,
-38.4719748427951,-37.4855139493901,-36.4990530559851,-35.5125921625801,
-35.2649009415391),.UNSPECIFIED.);
#170=B_SPLINE_CURVE_WITH_KNOTS('',3,(#9684,#9685,#9686,#9687,#9688,#9689,
#9690,#9691,#9692,#9693,#9694,#9695,#9696,#9697,#9698,#9699,#9700,#9701,
#9702,#9703,#9704,#9705),.UNSPECIFIED.,.F.,.F.,(4,3,3,3,3,3,3,4),(32.725489676875,
33.5396703757701,34.5261312691751,35.5125921625801,36.4990530559851,37.4855139493901,
38.4719748427951,39.0086749840546),.UNSPECIFIED.);
#171=B_SPLINE_CURVE_WITH_KNOTS('',3,(#9706,#9707,#9708,#9709,#9710,#9711,
#9712,#9713,#9714,#9715,#9716,#9717,#9718,#9719,#9720,#9721,#9722,#9723,
#9724,#9725,#9726,#9727),.UNSPECIFIED.,.F.,.F.,(4,3,3,3,3,3,3,4),(-35.2649009415391,
-34.5261312691751,-33.5396703757701,-32.5532094823651,-31.5667485889601,
-30.5802876955551,-29.5938268021501,-28.9817156343595),.UNSPECIFIED.);
#172=B_SPLINE_CURVE_WITH_KNOTS('',3,(#9732,#9733,#9734,#9735,#9736,#9737,
#9738,#9739,#9740,#9741,#9742,#9743,#9744,#9745,#9746,#9747,#9748,#9749,
#9750,#9751,#9752,#9753,#9754,#9755,#9756),.UNSPECIFIED.,.F.,.F.,(4,3,3,
3,3,3,3,3,4),(26.4423043696954,26.6344441219351,27.6209050153401,28.6073659087451,
29.5938268021501,30.5802876955551,31.5667485889601,32.5532094823651,32.725489676875),
 .UNSPECIFIED.);
#173=B_SPLINE_CURVE_WITH_KNOTS('',3,(#9757,#9758,#9759,#9760,#9761,#9762,
#9763,#9764,#9765,#9766,#9767,#9768,#9769,#9770,#9771,#9772,#9773,#9774,
#9775,#9776,#9777,#9778),.UNSPECIFIED.,.F.,.F.,(4,3,3,3,3,3,3,4),(-28.9817156343595,
-28.6073659087451,-27.6209050153401,-26.6344441219351,-25.6479832285301,
-24.6615223351251,-23.6750614417201,-22.6985303271799),.UNSPECIFIED.);
#174=B_SPLINE_CURVE_WITH_KNOTS('',3,(#9783,#9784,#9785,#9786,#9787,#9788,
#9789,#9790,#9791,#9792,#9793,#9794,#9795,#9796,#9797,#9798,#9799,#9800,
#9801,#9802,#9803,#9804),.UNSPECIFIED.,.F.,.F.,(4,3,3,3,3,3,3,4),(20.1591190625158,
20.7156787615051,21.7021396549101,22.6886005483151,23.6750614417201,24.6615223351251,
25.6479832285301,26.4423043696954),.UNSPECIFIED.);
#175=B_SPLINE_CURVE_WITH_KNOTS('',3,(#9805,#9806,#9807,#9808,#9809,#9810,
#9811,#9812,#9813,#9814,#9815,#9816,#9817,#9818,#9819,#9820,#9821,#9822,
#9823,#9824,#9825,#9826,#9827,#9828,#9829),.UNSPECIFIED.,.F.,.F.,(4,3,3,
3,3,3,3,3,4),(-22.6985303271799,-22.6886005483151,-21.7021396549101,-20.7156787615051,
-19.7292178681001,-18.7427569746951,-17.75629608129,-16.7698351878851,-16.4153450200003),
 .UNSPECIFIED.);
#176=B_SPLINE_CURVE_WITH_KNOTS('',3,(#9834,#9835,#9836,#9837,#9838,#9839,
#9840,#9841,#9842,#9843,#9844,#9845,#9846,#9847,#9848,#9849,#9850,#9851,
#9852,#9853,#9854,#9855),.UNSPECIFIED.,.F.,.F.,(4,3,3,3,3,3,3,4),(13.8759337553363,
14.796913401075,15.78337429448,16.769835187885,17.7562960812901,18.742756974695,
19.7292178681001,20.1591190625158),.UNSPECIFIED.);
#177=B_SPLINE_CURVE_WITH_KNOTS('',3,(#9856,#9857,#9858,#9859,#9860,#9861,
#9862,#9863,#9864,#9865,#9866,#9867,#9868,#9869,#9870,#9871,#9872,#9873,
#9874,#9875,#9876,#9877),.UNSPECIFIED.,.F.,.F.,(4,3,3,3,3,3,3,4),(-16.4153450200003,
-15.78337429448,-14.796913401075,-13.81045250767,-12.823991614265,-11.83753072086,
-10.851069827455,-10.1321597128207),.UNSPECIFIED.);
#178=B_SPLINE_CURVE_WITH_KNOTS('',3,(#9883,#9884,#9885,#9886,#9887,#9888,
#9889,#9890,#9891,#9892,#9893,#9894,#9895),.UNSPECIFIED.,.F.,.F.,(4,3,3,
3,4),(-3.84897440564113,-2.95938268021501,-1.97292178681,-0.986460893405001,
0.),.UNSPECIFIED.);
#179=B_SPLINE_CURVE_WITH_KNOTS('',3,(#9898,#9899,#9900,#9901,#9902,#9903,
#9904,#9905,#9906,#9907,#9908,#9909,#9910,#9911,#9912,#9913,#9914,#9915,
#9916),.UNSPECIFIED.,.F.,.F.,(4,3,3,3,3,3,4),(2.01694489302843,2.95938268021501,
3.94584357362001,4.93230446702501,5.91876536043002,6.90522625383502,7.59274844815667),
 .UNSPECIFIED.);
#180=B_SPLINE_CURVE_WITH_KNOTS('',3,(#9922,#9923,#9924,#9925),
 .UNSPECIFIED.,.F.,.F.,(4,4),(51.5750455984138,52.2824273504651),
 .UNSPECIFIED.);
#181=B_SPLINE_CURVE_WITH_KNOTS('',3,(#9928,#9929,#9930,#9931,#9932,#9933,
#9934,#9935,#9936,#9937),.UNSPECIFIED.,.F.,.F.,(4,3,3,4),(-50.2654824574367,
-49.3230446702501,-48.3365837768451,-47.8312715558982),.UNSPECIFIED.);
#182=B_SPLINE_CURVE_WITH_KNOTS('',3,(#9942,#9943,#9944,#9945,#9946,#9947,
#9948,#9949,#9950,#9951,#9952,#9953,#9954,#9955,#9956,#9957,#9958,#9959,
#9960,#9961,#9962,#9963,#9964,#9965,#9966),.UNSPECIFIED.,.F.,.F.,(4,3,3,
3,3,3,3,3,4),(45.2918602912342,45.3772010966301,46.3636619900351,47.3501228834401,
48.3365837768451,49.3230446702501,50.3095055636552,51.2959664570602,51.5750455984138),
 .UNSPECIFIED.);
#183=B_SPLINE_CURVE_WITH_KNOTS('',3,(#9967,#9968,#9969,#9970,#9971,#9972,
#9973,#9974,#9975,#9976,#9977,#9978,#9979,#9980,#9981,#9982,#9983,#9984,
#9985,#9986,#9987,#9988),.UNSPECIFIED.,.F.,.F.,(4,3,3,3,3,3,3,4),(-47.8312715558982,
-47.3501228834401,-46.3636619900351,-45.3772010966301,-44.3907402032251,
-43.4042793098201,-42.4178184164151,-41.5480862487187),.UNSPECIFIED.);
#184=B_SPLINE_CURVE_WITH_KNOTS('',3,(#9993,#9994,#9995,#9996,#9997,#9998,
#9999,#10000,#10001,#10002,#10003,#10004,#10005,#10006,#10007,#10008,#10009,
#10010,#10011,#10012,#10013,#10014),.UNSPECIFIED.,.F.,.F.,(4,3,3,3,3,3,
3,4),(39.0086749840546,39.4584357362001,40.4448966296051,41.4313575230101,
42.4178184164151,43.4042793098201,44.3907402032251,45.2918602912342),
 .UNSPECIFIED.);
#185=B_SPLINE_CURVE_WITH_KNOTS('',3,(#10015,#10016,#10017,#10018,#10019,
#10020,#10021,#10022,#10023,#10024,#10025,#10026,#10027,#10028,#10029,#10030,
#10031,#10032,#10033,#10034,#10035,#10036,#10037,#10038,#10039),
 .UNSPECIFIED.,.F.,.F.,(4,3,3,3,3,3,3,3,4),(-41.5480862487187,-41.4313575230101,
-40.4448966296051,-39.4584357362001,-38.4719748427951,-37.4855139493901,
-36.4990530559851,-35.5125921625801,-35.2649009415391),.UNSPECIFIED.);
#186=B_SPLINE_CURVE_WITH_KNOTS('',3,(#10044,#10045,#10046,#10047,#10048,
#10049,#10050,#10051,#10052,#10053,#10054,#10055,#10056,#10057,#10058,#10059,
#10060,#10061,#10062,#10063,#10064,#10065),.UNSPECIFIED.,.F.,.F.,(4,3,3,
3,3,3,3,4),(32.725489676875,33.5396703757701,34.5261312691751,35.5125921625801,
36.4990530559851,37.4855139493901,38.4719748427951,39.0086749840546),
 .UNSPECIFIED.);
#187=B_SPLINE_CURVE_WITH_KNOTS('',3,(#10066,#10067,#10068,#10069,#10070,
#10071,#10072,#10073,#10074,#10075,#10076,#10077,#10078,#10079,#10080,#10081,
#10082,#10083,#10084,#10085,#10086,#10087),.UNSPECIFIED.,.F.,.F.,(4,3,3,
3,3,3,3,4),(-35.2649009415391,-34.5261312691751,-33.5396703757701,-32.5532094823651,
-31.5667485889601,-30.5802876955551,-29.5938268021501,-28.9817156343595),
 .UNSPECIFIED.);
#188=B_SPLINE_CURVE_WITH_KNOTS('',3,(#10092,#10093,#10094,#10095,#10096,
#10097,#10098,#10099,#10100,#10101,#10102,#10103,#10104,#10105,#10106,#10107,
#10108,#10109,#10110,#10111,#10112,#10113,#10114,#10115,#10116),
 .UNSPECIFIED.,.F.,.F.,(4,3,3,3,3,3,3,3,4),(26.4423043696954,26.6344441219351,
27.6209050153401,28.6073659087451,29.5938268021501,30.5802876955551,31.5667485889601,
32.5532094823651,32.725489676875),.UNSPECIFIED.);
#189=B_SPLINE_CURVE_WITH_KNOTS('',3,(#10117,#10118,#10119,#10120,#10121,
#10122,#10123,#10124,#10125,#10126,#10127,#10128,#10129,#10130,#10131,#10132,
#10133,#10134,#10135,#10136,#10137,#10138),.UNSPECIFIED.,.F.,.F.,(4,3,3,
3,3,3,3,4),(-28.9817156343595,-28.6073659087451,-27.6209050153401,-26.6344441219351,
-25.6479832285301,-24.6615223351251,-23.6750614417201,-22.6985303271799),
 .UNSPECIFIED.);
#190=B_SPLINE_CURVE_WITH_KNOTS('',3,(#10143,#10144,#10145,#10146,#10147,
#10148,#10149,#10150,#10151,#10152,#10153,#10154,#10155,#10156,#10157,#10158,
#10159,#10160,#10161,#10162,#10163,#10164),.UNSPECIFIED.,.F.,.F.,(4,3,3,
3,3,3,3,4),(20.1591190625158,20.7156787615051,21.7021396549101,22.6886005483151,
23.6750614417201,24.6615223351251,25.6479832285301,26.4423043696954),
 .UNSPECIFIED.);
#191=B_SPLINE_CURVE_WITH_KNOTS('',3,(#10165,#10166,#10167,#10168,#10169,
#10170,#10171,#10172,#10173,#10174,#10175,#10176,#10177,#10178,#10179,#10180,
#10181,#10182,#10183,#10184,#10185,#10186,#10187,#10188,#10189),
 .UNSPECIFIED.,.F.,.F.,(4,3,3,3,3,3,3,3,4),(-22.6985303271799,-22.6886005483151,
-21.7021396549101,-20.7156787615051,-19.7292178681001,-18.7427569746951,
-17.75629608129,-16.769835187885,-16.4153450200003),.UNSPECIFIED.);
#192=B_SPLINE_CURVE_WITH_KNOTS('',3,(#10194,#10195,#10196,#10197,#10198,
#10199,#10200,#10201,#10202,#10203,#10204,#10205,#10206,#10207,#10208,#10209,
#10210,#10211,#10212,#10213,#10214,#10215),.UNSPECIFIED.,.F.,.F.,(4,3,3,
3,3,3,3,4),(13.8759337553363,14.796913401075,15.78337429448,16.769835187885,
17.7562960812901,18.742756974695,19.7292178681001,20.1591190625158),
 .UNSPECIFIED.);
#193=B_SPLINE_CURVE_WITH_KNOTS('',3,(#10216,#10217,#10218,#10219,#10220,
#10221,#10222,#10223,#10224,#10225,#10226,#10227,#10228,#10229,#10230,#10231,
#10232,#10233,#10234,#10235,#10236,#10237),.UNSPECIFIED.,.F.,.F.,(4,3,3,
3,3,3,3,4),(-16.4153450200003,-15.78337429448,-14.796913401075,-13.81045250767,
-12.823991614265,-11.83753072086,-10.851069827455,-10.1321597128207),
 .UNSPECIFIED.);
#194=B_SPLINE_CURVE_WITH_KNOTS('',3,(#10243,#10244,#10245,#10246,#10247,
#10248,#10249,#10250,#10251,#10252,#10253,#10254,#10255),.UNSPECIFIED.,
 .F.,.F.,(4,3,3,3,4),(-3.84897440564114,-2.95938268021501,-1.97292178681001,
-0.986460893405003,0.),.UNSPECIFIED.);
#195=B_SPLINE_CURVE_WITH_KNOTS('',3,(#10258,#10259,#10260,#10261,#10262,
#10263,#10264,#10265,#10266,#10267,#10268,#10269,#10270,#10271,#10272,#10273,
#10274,#10275,#10276),.UNSPECIFIED.,.F.,.F.,(4,3,3,3,3,3,4),(2.01694489302845,
2.95938268021501,3.94584357362001,4.93230446702501,5.91876536043002,6.90522625383502,
7.59274844815667),.UNSPECIFIED.);
#196=B_SPLINE_CURVE_WITH_KNOTS('',3,(#10282,#10283,#10284,#10285),
 .UNSPECIFIED.,.F.,.F.,(4,4),(51.5750455984138,52.2824273504651),
 .UNSPECIFIED.);
#197=B_SPLINE_CURVE_WITH_KNOTS('',3,(#10288,#10289,#10290,#10291,#10292,
#10293,#10294,#10295,#10296,#10297),.UNSPECIFIED.,.F.,.F.,(4,3,3,4),(-50.2654824574367,
-49.3230446702501,-48.3365837768451,-47.8312715558982),.UNSPECIFIED.);
#198=B_SPLINE_CURVE_WITH_KNOTS('',3,(#10302,#10303,#10304,#10305,#10306,
#10307,#10308,#10309,#10310,#10311,#10312,#10313,#10314,#10315,#10316,#10317,
#10318,#10319,#10320,#10321,#10322,#10323,#10324,#10325,#10326),
 .UNSPECIFIED.,.F.,.F.,(4,3,3,3,3,3,3,3,4),(45.2918602912342,45.3772010966301,
46.3636619900351,47.3501228834401,48.3365837768451,49.3230446702501,50.3095055636551,
51.2959664570601,51.5750455984138),.UNSPECIFIED.);
#199=B_SPLINE_CURVE_WITH_KNOTS('',3,(#10327,#10328,#10329,#10330,#10331,
#10332,#10333,#10334,#10335,#10336,#10337,#10338,#10339,#10340,#10341,#10342,
#10343,#10344,#10345,#10346,#10347,#10348),.UNSPECIFIED.,.F.,.F.,(4,3,3,
3,3,3,3,4),(-47.8312715558982,-47.3501228834401,-46.3636619900351,-45.3772010966301,
-44.3907402032251,-43.4042793098201,-42.4178184164151,-41.5480862487187),
 .UNSPECIFIED.);
#200=B_SPLINE_CURVE_WITH_KNOTS('',3,(#10353,#10354,#10355,#10356,#10357,
#10358,#10359,#10360,#10361,#10362,#10363,#10364,#10365,#10366,#10367,#10368,
#10369,#10370,#10371,#10372,#10373,#10374),.UNSPECIFIED.,.F.,.F.,(4,3,3,
3,3,3,3,4),(39.0086749840546,39.4584357362001,40.4448966296051,41.4313575230101,
42.4178184164151,43.4042793098201,44.3907402032251,45.2918602912342),
 .UNSPECIFIED.);
#201=B_SPLINE_CURVE_WITH_KNOTS('',3,(#10375,#10376,#10377,#10378,#10379,
#10380,#10381,#10382,#10383,#10384,#10385,#10386,#10387,#10388,#10389,#10390,
#10391,#10392,#10393,#10394,#10395,#10396,#10397,#10398,#10399),
 .UNSPECIFIED.,.F.,.F.,(4,3,3,3,3,3,3,3,4),(-41.5480862487187,-41.4313575230101,
-40.4448966296051,-39.4584357362001,-38.4719748427951,-37.4855139493901,
-36.4990530559851,-35.5125921625801,-35.2649009415391),.UNSPECIFIED.);
#202=B_SPLINE_CURVE_WITH_KNOTS('',3,(#10404,#10405,#10406,#10407,#10408,
#10409,#10410,#10411,#10412,#10413,#10414,#10415,#10416,#10417,#10418,#10419,
#10420,#10421,#10422,#10423,#10424,#10425),.UNSPECIFIED.,.F.,.F.,(4,3,3,
3,3,3,3,4),(32.725489676875,33.5396703757701,34.5261312691751,35.5125921625801,
36.4990530559851,37.4855139493901,38.4719748427951,39.0086749840546),
 .UNSPECIFIED.);
#203=B_SPLINE_CURVE_WITH_KNOTS('',3,(#10426,#10427,#10428,#10429,#10430,
#10431,#10432,#10433,#10434,#10435,#10436,#10437,#10438,#10439,#10440,#10441,
#10442,#10443,#10444,#10445,#10446,#10447),.UNSPECIFIED.,.F.,.F.,(4,3,3,
3,3,3,3,4),(-35.2649009415391,-34.5261312691751,-33.5396703757701,-32.5532094823651,
-31.5667485889601,-30.5802876955551,-29.5938268021501,-28.9817156343595),
 .UNSPECIFIED.);
#204=B_SPLINE_CURVE_WITH_KNOTS('',3,(#10452,#10453,#10454,#10455,#10456,
#10457,#10458,#10459,#10460,#10461,#10462,#10463,#10464,#10465,#10466,#10467,
#10468,#10469,#10470,#10471,#10472,#10473,#10474,#10475,#10476),
 .UNSPECIFIED.,.F.,.F.,(4,3,3,3,3,3,3,3,4),(26.4423043696954,26.6344441219351,
27.6209050153401,28.6073659087451,29.5938268021501,30.5802876955551,31.5667485889601,
32.5532094823651,32.725489676875),.UNSPECIFIED.);
#205=B_SPLINE_CURVE_WITH_KNOTS('',3,(#10477,#10478,#10479,#10480,#10481,
#10482,#10483,#10484,#10485,#10486,#10487,#10488,#10489,#10490,#10491,#10492,
#10493,#10494,#10495,#10496,#10497,#10498),.UNSPECIFIED.,.F.,.F.,(4,3,3,
3,3,3,3,4),(-28.9817156343595,-28.6073659087451,-27.6209050153401,-26.6344441219351,
-25.6479832285301,-24.6615223351251,-23.6750614417201,-22.6985303271799),
 .UNSPECIFIED.);
#206=B_SPLINE_CURVE_WITH_KNOTS('',3,(#10503,#10504,#10505,#10506,#10507,
#10508,#10509,#10510,#10511,#10512,#10513,#10514,#10515,#10516,#10517,#10518,
#10519,#10520,#10521,#10522,#10523,#10524),.UNSPECIFIED.,.F.,.F.,(4,3,3,
3,3,3,3,4),(20.1591190625158,20.7156787615051,21.7021396549101,22.6886005483151,
23.6750614417201,24.6615223351251,25.6479832285301,26.4423043696954),
 .UNSPECIFIED.);
#207=B_SPLINE_CURVE_WITH_KNOTS('',3,(#10525,#10526,#10527,#10528,#10529,
#10530,#10531,#10532,#10533,#10534,#10535,#10536,#10537,#10538,#10539,#10540,
#10541,#10542,#10543,#10544,#10545,#10546,#10547,#10548,#10549),
 .UNSPECIFIED.,.F.,.F.,(4,3,3,3,3,3,3,3,4),(-22.6985303271799,-22.6886005483151,
-21.7021396549101,-20.7156787615051,-19.7292178681001,-18.7427569746951,
-17.75629608129,-16.769835187885,-16.4153450200003),.UNSPECIFIED.);
#208=B_SPLINE_CURVE_WITH_KNOTS('',3,(#10554,#10555,#10556,#10557,#10558,
#10559,#10560,#10561,#10562,#10563,#10564,#10565,#10566,#10567,#10568,#10569,
#10570,#10571,#10572,#10573,#10574,#10575),.UNSPECIFIED.,.F.,.F.,(4,3,3,
3,3,3,3,4),(13.8759337553363,14.796913401075,15.78337429448,16.769835187885,
17.7562960812901,18.742756974695,19.7292178681001,20.1591190625158),
 .UNSPECIFIED.);
#209=B_SPLINE_CURVE_WITH_KNOTS('',3,(#10576,#10577,#10578,#10579,#10580,
#10581,#10582,#10583,#10584,#10585,#10586,#10587,#10588,#10589,#10590,#10591,
#10592,#10593,#10594,#10595,#10596,#10597),.UNSPECIFIED.,.F.,.F.,(4,3,3,
3,3,3,3,4),(-16.4153450200003,-15.78337429448,-14.796913401075,-13.81045250767,
-12.823991614265,-11.83753072086,-10.851069827455,-10.1321597128207),
 .UNSPECIFIED.);
#210=B_SPLINE_CURVE_WITH_KNOTS('',3,(#10603,#10604,#10605,#10606,#10607,
#10608,#10609,#10610,#10611,#10612,#10613,#10614,#10615),.UNSPECIFIED.,
 .F.,.F.,(4,3,3,3,4),(-3.84897440564114,-2.95938268021501,-1.97292178681001,
-0.986460893405003,0.),.UNSPECIFIED.);
#211=B_SPLINE_CURVE_WITH_KNOTS('',3,(#10618,#10619,#10620,#10621,#10622,
#10623,#10624,#10625,#10626,#10627,#10628,#10629,#10630,#10631,#10632,#10633,
#10634,#10635,#10636),.UNSPECIFIED.,.F.,.F.,(4,3,3,3,3,3,4),(2.01694489302845,
2.95938268021501,3.94584357362001,4.93230446702501,5.91876536043002,6.90522625383502,
7.59274844815667),.UNSPECIFIED.);
#212=B_SPLINE_CURVE_WITH_KNOTS('',3,(#10642,#10643,#10644,#10645,#10646,
#10647,#10648,#10649),.UNSPECIFIED.,.F.,.F.,(4,1,1,1,1,4),(59.6902604182061,
60.195572639153,61.182033532558,62.168494425963,63.154955319368,64.141416212773),
 .UNSPECIFIED.);
#213=B_SPLINE_CURVE_WITH_KNOTS('',3,(#10652,#10653,#10654,#10655,#10656,
#10657,#10658,#10659,#10660),.UNSPECIFIED.,.F.,.F.,(4,1,1,1,1,1,4),(59.6902604182061,
59.775601223602,60.762062117007,61.748523010412,62.734983903817,63.721444797222,
64.6638825844085),.UNSPECIFIED.);
#214=B_SPLINE_CURVE_WITH_KNOTS('',3,(#10665,#10666,#10667,#10668,#10669,
#10670,#10671,#10672,#10673,#10674),.UNSPECIFIED.,.F.,.F.,(4,1,1,1,1,1,
1,4),(53.4070751110265,54.2768072787229,55.2632681721279,56.2497290655329,
57.2361899589379,58.222650852343,59.209111745748,59.6902604182061),
 .UNSPECIFIED.);
#215=B_SPLINE_CURVE_WITH_KNOTS('',3,(#10675,#10676,#10677,#10678,#10679,
#10680,#10681,#10682,#10683,#10684),.UNSPECIFIED.,.F.,.F.,(4,1,1,1,1,1,
1,4),(53.4070751110265,53.856835863172,54.843296756577,55.829757649982,
56.816218543387,57.802679436792,58.789140330197,59.6902604182061),
 .UNSPECIFIED.);
#216=B_SPLINE_CURVE_WITH_KNOTS('',3,(#10689,#10690,#10691,#10692,#10693,
#10694,#10695,#10696,#10697,#10698,#10699),.UNSPECIFIED.,.F.,.F.,(4,1,1,
1,1,1,1,1,4),(47.1238898038469,47.3715810248879,48.3580419182929,49.3445028116979,
50.3309637051029,51.3174245985079,52.3038854919129,53.2903463853179,53.4070751110265),
 .UNSPECIFIED.);
#217=B_SPLINE_CURVE_WITH_KNOTS('',3,(#10700,#10701,#10702,#10703,#10704,
#10705,#10706,#10707,#10708,#10709),.UNSPECIFIED.,.F.,.F.,(4,1,1,1,1,1,
1,4),(47.1238898038469,47.9380705027419,48.9245313961469,49.9109922895519,
50.8974531829569,51.8839140763619,52.8703749697669,53.4070751110265),
 .UNSPECIFIED.);
#218=B_SPLINE_CURVE_WITH_KNOTS('',3,(#10714,#10715,#10716,#10717,#10718,
#10719,#10720,#10721,#10722,#10723),.UNSPECIFIED.,.F.,.F.,(4,1,1,1,1,1,
1,4),(40.8407044966673,41.4528156644579,42.4392765578629,43.4257374512679,
44.4121983446729,45.3986592380779,46.3851201314829,47.1238898038469),
 .UNSPECIFIED.);
#219=B_SPLINE_CURVE_WITH_KNOTS('',3,(#10724,#10725,#10726,#10727,#10728,
#10729,#10730,#10731,#10732,#10733,#10734),.UNSPECIFIED.,.F.,.F.,(4,1,1,
1,1,1,1,1,4),(40.8407044966673,41.0328442489069,42.0193051423119,43.0057660357169,
43.9922269291219,44.9786878225269,45.9651487159319,46.9516096093369,47.1238898038469),
 .UNSPECIFIED.);
#220=B_SPLINE_CURVE_WITH_KNOTS('',3,(#10739,#10740,#10741,#10742,#10743,
#10744,#10745,#10746,#10747,#10748),.UNSPECIFIED.,.F.,.F.,(4,1,1,1,1,1,
1,4),(34.5575191894877,35.5340503040279,36.5205111974329,37.5069720908379,
38.4934329842429,39.4798938776479,40.4663547710529,40.8407044966673),
 .UNSPECIFIED.);
#221=B_SPLINE_CURVE_WITH_KNOTS('',3,(#10749,#10750,#10751,#10752,#10753,
#10754,#10755,#10756,#10757,#10758),.UNSPECIFIED.,.F.,.F.,(4,1,1,1,1,1,
1,4),(34.5575191894877,35.1140788884769,36.1005397818819,37.0870006752869,
38.0734615686919,39.0599224620969,40.0463833555019,40.8407044966673),
 .UNSPECIFIED.);
#222=B_SPLINE_CURVE_WITH_KNOTS('',3,(#10763,#10764,#10765,#10766,#10767,
#10768,#10769,#10770,#10771,#10772,#10773),.UNSPECIFIED.,.F.,.F.,(4,1,1,
1,1,1,1,1,4),(28.2743338823081,28.6288240501929,29.6152849435979,30.6017458370029,
31.5882067304079,32.5746676238129,33.5611285172179,34.5475894106229,34.5575191894877),
 .UNSPECIFIED.);
#223=B_SPLINE_CURVE_WITH_KNOTS('',3,(#10774,#10775,#10776,#10777,#10778,
#10779,#10780,#10781,#10782,#10783),.UNSPECIFIED.,.F.,.F.,(4,1,1,1,1,1,
1,4),(28.2743338823081,29.1953135280469,30.1817744214519,31.1682353148569,
32.1546962082619,33.1411571016669,34.1276179950719,34.5575191894877),
 .UNSPECIFIED.);
#224=B_SPLINE_CURVE_WITH_KNOTS('',3,(#10788,#10789,#10790,#10791,#10792,
#10793,#10794,#10795,#10796,#10797),.UNSPECIFIED.,.F.,.F.,(4,1,1,1,1,1,
1,4),(21.9911485751285,22.7100586897628,23.6965195831678,24.6829804765729,
25.6694413699779,26.6559022633829,27.6423631567879,28.2743338823081),
 .UNSPECIFIED.);
#225=B_SPLINE_CURVE_WITH_KNOTS('',3,(#10798,#10799,#10800,#10801,#10802,
#10803,#10804,#10805,#10806,#10807,#10808),.UNSPECIFIED.,.F.,.F.,(4,1,1,
1,1,1,1,1,4),(21.9911485751285,22.2900872742119,23.2765481676169,24.2630090610219,
25.2494699544269,26.2359308478319,27.2223917412369,28.2088526346419,28.2743338823081),
 .UNSPECIFIED.);
#226=B_SPLINE_CURVE_WITH_KNOTS('',3,(#10814,#10815,#10816,#10817,#10818),
 .UNSPECIFIED.,.F.,.F.,(4,1,4),(14.3984001269718,15.3848610203768,15.7079632679489),
 .UNSPECIFIED.);
#227=B_SPLINE_CURVE_WITH_KNOTS('',3,(#10821,#10822,#10823,#10824,#10825),
 .UNSPECIFIED.,.F.,.F.,(4,1,4),(13.8759337553363,14.8183715425228,15.7079632679489),
 .UNSPECIFIED.);
#228=B_SPLINE_CURVE_WITH_KNOTS('',3,(#10831,#10832,#10833,#10834,#10835,
#10836,#10837,#10838),.UNSPECIFIED.,.F.,.F.,(4,1,1,1,1,4),(59.6902604182061,
60.1955726391529,61.1820335325579,62.1684944259629,63.154955319368,64.141416212773),
 .UNSPECIFIED.);
#229=B_SPLINE_CURVE_WITH_KNOTS('',3,(#10841,#10842,#10843,#10844,#10845,
#10846,#10847,#10848,#10849),.UNSPECIFIED.,.F.,.F.,(4,1,1,1,1,1,4),(59.6902604182061,
59.775601223602,60.762062117007,61.748523010412,62.734983903817,63.721444797222,
64.6638825844085),.UNSPECIFIED.);
#230=B_SPLINE_CURVE_WITH_KNOTS('',3,(#10854,#10855,#10856,#10857,#10858,
#10859,#10860,#10861,#10862,#10863),.UNSPECIFIED.,.F.,.F.,(4,1,1,1,1,1,
1,4),(53.4070751110265,54.2768072787229,55.2632681721279,56.2497290655329,
57.2361899589379,58.2226508523429,59.2091117457479,59.6902604182061),
 .UNSPECIFIED.);
#231=B_SPLINE_CURVE_WITH_KNOTS('',3,(#10864,#10865,#10866,#10867,#10868,
#10869,#10870,#10871,#10872,#10873),.UNSPECIFIED.,.F.,.F.,(4,1,1,1,1,1,
1,4),(53.4070751110265,53.856835863172,54.843296756577,55.829757649982,
56.816218543387,57.802679436792,58.789140330197,59.6902604182061),
 .UNSPECIFIED.);
#232=B_SPLINE_CURVE_WITH_KNOTS('',3,(#10878,#10879,#10880,#10881,#10882,
#10883,#10884,#10885,#10886,#10887,#10888),.UNSPECIFIED.,.F.,.F.,(4,1,1,
1,1,1,1,1,4),(47.1238898038469,47.3715810248879,48.3580419182929,49.3445028116979,
50.3309637051029,51.3174245985079,52.3038854919129,53.2903463853179,53.4070751110265),
 .UNSPECIFIED.);
#233=B_SPLINE_CURVE_WITH_KNOTS('',3,(#10889,#10890,#10891,#10892,#10893,
#10894,#10895,#10896,#10897,#10898),.UNSPECIFIED.,.F.,.F.,(4,1,1,1,1,1,
1,4),(47.1238898038469,47.9380705027419,48.9245313961469,49.9109922895519,
50.8974531829569,51.8839140763619,52.8703749697669,53.4070751110265),
 .UNSPECIFIED.);
#234=B_SPLINE_CURVE_WITH_KNOTS('',3,(#10903,#10904,#10905,#10906,#10907,
#10908,#10909,#10910,#10911,#10912),.UNSPECIFIED.,.F.,.F.,(4,1,1,1,1,1,
1,4),(40.8407044966673,41.4528156644579,42.4392765578629,43.4257374512679,
44.4121983446729,45.3986592380779,46.3851201314829,47.1238898038469),
 .UNSPECIFIED.);
#235=B_SPLINE_CURVE_WITH_KNOTS('',3,(#10913,#10914,#10915,#10916,#10917,
#10918,#10919,#10920,#10921,#10922,#10923),.UNSPECIFIED.,.F.,.F.,(4,1,1,
1,1,1,1,1,4),(40.8407044966673,41.0328442489069,42.0193051423119,43.0057660357169,
43.9922269291219,44.9786878225269,45.9651487159319,46.9516096093369,47.1238898038469),
 .UNSPECIFIED.);
#236=B_SPLINE_CURVE_WITH_KNOTS('',3,(#10928,#10929,#10930,#10931,#10932,
#10933,#10934,#10935,#10936,#10937),.UNSPECIFIED.,.F.,.F.,(4,1,1,1,1,1,
1,4),(34.5575191894877,35.5340503040279,36.5205111974329,37.5069720908379,
38.4934329842429,39.4798938776479,40.4663547710529,40.8407044966673),
 .UNSPECIFIED.);
#237=B_SPLINE_CURVE_WITH_KNOTS('',3,(#10938,#10939,#10940,#10941,#10942,
#10943,#10944,#10945,#10946,#10947),.UNSPECIFIED.,.F.,.F.,(4,1,1,1,1,1,
1,4),(34.5575191894877,35.1140788884769,36.1005397818819,37.0870006752869,
38.0734615686919,39.0599224620969,40.0463833555019,40.8407044966673),
 .UNSPECIFIED.);
#238=B_SPLINE_CURVE_WITH_KNOTS('',3,(#10952,#10953,#10954,#10955,#10956,
#10957,#10958,#10959,#10960,#10961,#10962),.UNSPECIFIED.,.F.,.F.,(4,1,1,
1,1,1,1,1,4),(28.2743338823081,28.6288240501929,29.6152849435979,30.6017458370029,
31.5882067304079,32.5746676238129,33.5611285172179,34.5475894106229,34.5575191894877),
 .UNSPECIFIED.);
#239=B_SPLINE_CURVE_WITH_KNOTS('',3,(#10963,#10964,#10965,#10966,#10967,
#10968,#10969,#10970,#10971,#10972),.UNSPECIFIED.,.F.,.F.,(4,1,1,1,1,1,
1,4),(28.2743338823081,29.1953135280469,30.1817744214519,31.1682353148569,
32.1546962082619,33.1411571016669,34.1276179950719,34.5575191894877),
 .UNSPECIFIED.);
#240=B_SPLINE_CURVE_WITH_KNOTS('',3,(#10977,#10978,#10979,#10980,#10981,
#10982,#10983,#10984,#10985,#10986),.UNSPECIFIED.,.F.,.F.,(4,1,1,1,1,1,
1,4),(21.9911485751285,22.7100586897628,23.6965195831678,24.6829804765728,
25.6694413699778,26.6559022633828,27.6423631567879,28.2743338823081),
 .UNSPECIFIED.);
#241=B_SPLINE_CURVE_WITH_KNOTS('',3,(#10987,#10988,#10989,#10990,#10991,
#10992,#10993,#10994,#10995,#10996,#10997),.UNSPECIFIED.,.F.,.F.,(4,1,1,
1,1,1,1,1,4),(21.9911485751285,22.2900872742119,23.2765481676169,24.2630090610219,
25.2494699544269,26.2359308478319,27.2223917412369,28.2088526346419,28.2743338823081),
 .UNSPECIFIED.);
#242=B_SPLINE_CURVE_WITH_KNOTS('',3,(#11003,#11004,#11005,#11006,#11007),
 .UNSPECIFIED.,.F.,.F.,(4,1,4),(14.3984001269718,15.3848610203768,15.7079632679489),
 .UNSPECIFIED.);
#243=B_SPLINE_CURVE_WITH_KNOTS('',3,(#11010,#11011,#11012,#11013,#11014),
 .UNSPECIFIED.,.F.,.F.,(4,1,4),(13.8759337553363,14.8183715425228,15.7079632679489),
 .UNSPECIFIED.);
#244=B_SPLINE_CURVE_WITH_KNOTS('',3,(#11020,#11021,#11022,#11023,#11024,
#11025,#11026,#11027),.UNSPECIFIED.,.F.,.F.,(4,1,1,1,1,4),(59.6902604182061,
60.1955726391529,61.1820335325579,62.1684944259629,63.154955319368,64.141416212773),
 .UNSPECIFIED.);
#245=B_SPLINE_CURVE_WITH_KNOTS('',3,(#11030,#11031,#11032,#11033,#11034,
#11035,#11036,#11037,#11038),.UNSPECIFIED.,.F.,.F.,(4,1,1,1,1,1,4),(59.6902604182061,
59.775601223602,60.762062117007,61.748523010412,62.734983903817,63.721444797222,
64.6638825844085),.UNSPECIFIED.);
#246=B_SPLINE_CURVE_WITH_KNOTS('',3,(#11043,#11044,#11045,#11046,#11047,
#11048,#11049,#11050,#11051,#11052),.UNSPECIFIED.,.F.,.F.,(4,1,1,1,1,1,
1,4),(53.4070751110265,54.2768072787229,55.2632681721279,56.2497290655329,
57.2361899589379,58.2226508523429,59.2091117457479,59.6902604182061),
 .UNSPECIFIED.);
#247=B_SPLINE_CURVE_WITH_KNOTS('',3,(#11053,#11054,#11055,#11056,#11057,
#11058,#11059,#11060,#11061,#11062),.UNSPECIFIED.,.F.,.F.,(4,1,1,1,1,1,
1,4),(53.4070751110265,53.8568358631719,54.8432967565769,55.8297576499819,
56.816218543387,57.802679436792,58.789140330197,59.6902604182061),
 .UNSPECIFIED.);
#248=B_SPLINE_CURVE_WITH_KNOTS('',3,(#11067,#11068,#11069,#11070,#11071,
#11072,#11073,#11074,#11075,#11076,#11077),.UNSPECIFIED.,.F.,.F.,(4,1,1,
1,1,1,1,1,4),(47.1238898038469,47.3715810248879,48.3580419182929,49.3445028116979,
50.3309637051029,51.3174245985079,52.3038854919129,53.2903463853179,53.4070751110265),
 .UNSPECIFIED.);
#249=B_SPLINE_CURVE_WITH_KNOTS('',3,(#11078,#11079,#11080,#11081,#11082,
#11083,#11084,#11085,#11086,#11087),.UNSPECIFIED.,.F.,.F.,(4,1,1,1,1,1,
1,4),(47.1238898038469,47.9380705027419,48.9245313961469,49.9109922895519,
50.8974531829569,51.8839140763619,52.8703749697669,53.4070751110265),
 .UNSPECIFIED.);
#250=B_SPLINE_CURVE_WITH_KNOTS('',3,(#11092,#11093,#11094,#11095,#11096,
#11097,#11098,#11099,#11100,#11101),.UNSPECIFIED.,.F.,.F.,(4,1,1,1,1,1,
1,4),(40.8407044966673,41.4528156644579,42.4392765578629,43.4257374512679,
44.4121983446729,45.3986592380779,46.3851201314829,47.1238898038469),
 .UNSPECIFIED.);
#251=B_SPLINE_CURVE_WITH_KNOTS('',3,(#11102,#11103,#11104,#11105,#11106,
#11107,#11108,#11109,#11110,#11111,#11112),.UNSPECIFIED.,.F.,.F.,(4,1,1,
1,1,1,1,1,4),(40.8407044966673,41.0328442489069,42.0193051423119,43.0057660357169,
43.9922269291219,44.9786878225269,45.9651487159319,46.9516096093369,47.1238898038469),
 .UNSPECIFIED.);
#252=B_SPLINE_CURVE_WITH_KNOTS('',3,(#11117,#11118,#11119,#11120,#11121,
#11122,#11123,#11124,#11125,#11126),.UNSPECIFIED.,.F.,.F.,(4,1,1,1,1,1,
1,4),(34.5575191894877,35.5340503040279,36.5205111974329,37.5069720908379,
38.4934329842429,39.4798938776479,40.4663547710529,40.8407044966673),
 .UNSPECIFIED.);
#253=B_SPLINE_CURVE_WITH_KNOTS('',3,(#11127,#11128,#11129,#11130,#11131,
#11132,#11133,#11134,#11135,#11136),.UNSPECIFIED.,.F.,.F.,(4,1,1,1,1,1,
1,4),(34.5575191894877,35.1140788884769,36.1005397818819,37.0870006752869,
38.0734615686919,39.0599224620969,40.0463833555019,40.8407044966673),
 .UNSPECIFIED.);
#254=B_SPLINE_CURVE_WITH_KNOTS('',3,(#11141,#11142,#11143,#11144,#11145,
#11146,#11147,#11148,#11149,#11150,#11151),.UNSPECIFIED.,.F.,.F.,(4,1,1,
1,1,1,1,1,4),(28.2743338823081,28.6288240501929,29.6152849435979,30.6017458370029,
31.5882067304079,32.5746676238129,33.5611285172179,34.5475894106229,34.5575191894877),
 .UNSPECIFIED.);
#255=B_SPLINE_CURVE_WITH_KNOTS('',3,(#11152,#11153,#11154,#11155,#11156,
#11157,#11158,#11159,#11160,#11161),.UNSPECIFIED.,.F.,.F.,(4,1,1,1,1,1,
1,4),(28.2743338823081,29.1953135280469,30.1817744214519,31.1682353148569,
32.1546962082619,33.1411571016669,34.1276179950719,34.5575191894877),
 .UNSPECIFIED.);
#256=B_SPLINE_CURVE_WITH_KNOTS('',3,(#11166,#11167,#11168,#11169,#11170,
#11171,#11172,#11173,#11174,#11175),.UNSPECIFIED.,.F.,.F.,(4,1,1,1,1,1,
1,4),(21.9911485751285,22.7100586897628,23.6965195831678,24.6829804765728,
25.6694413699778,26.6559022633828,27.6423631567879,28.2743338823081),
 .UNSPECIFIED.);
#257=B_SPLINE_CURVE_WITH_KNOTS('',3,(#11176,#11177,#11178,#11179,#11180,
#11181,#11182,#11183,#11184,#11185,#11186),.UNSPECIFIED.,.F.,.F.,(4,1,1,
1,1,1,1,1,4),(21.9911485751285,22.2900872742119,23.2765481676169,24.2630090610219,
25.2494699544269,26.2359308478319,27.2223917412369,28.2088526346419,28.2743338823081),
 .UNSPECIFIED.);
#258=B_SPLINE_CURVE_WITH_KNOTS('',3,(#11192,#11193,#11194,#11195,#11196),
 .UNSPECIFIED.,.F.,.F.,(4,1,4),(14.3984001269718,15.3848610203768,15.7079632679489),
 .UNSPECIFIED.);
#259=B_SPLINE_CURVE_WITH_KNOTS('',3,(#11199,#11200,#11201,#11202,#11203),
 .UNSPECIFIED.,.F.,.F.,(4,1,4),(13.8759337553363,14.8183715425228,15.7079632679489),
 .UNSPECIFIED.);
#260=B_SPLINE_CURVE_WITH_KNOTS('',3,(#11209,#11210,#11211,#11212,#11213,
#11214,#11215,#11216),.UNSPECIFIED.,.F.,.F.,(4,1,1,1,1,4),(59.6902604182061,
60.195572639153,61.182033532558,62.168494425963,63.154955319368,64.141416212773),
 .UNSPECIFIED.);
#261=B_SPLINE_CURVE_WITH_KNOTS('',3,(#11219,#11220,#11221,#11222,#11223,
#11224,#11225,#11226,#11227),.UNSPECIFIED.,.F.,.F.,(4,1,1,1,1,1,4),(59.6902604182061,
59.775601223602,60.762062117007,61.748523010412,62.734983903817,63.721444797222,
64.6638825844085),.UNSPECIFIED.);
#262=B_SPLINE_CURVE_WITH_KNOTS('',3,(#11232,#11233,#11234,#11235,#11236,
#11237,#11238,#11239,#11240,#11241),.UNSPECIFIED.,.F.,.F.,(4,1,1,1,1,1,
1,4),(53.4070751110265,54.2768072787229,55.2632681721279,56.2497290655329,
57.2361899589379,58.222650852343,59.209111745748,59.6902604182061),
 .UNSPECIFIED.);
#263=B_SPLINE_CURVE_WITH_KNOTS('',3,(#11242,#11243,#11244,#11245,#11246,
#11247,#11248,#11249,#11250,#11251),.UNSPECIFIED.,.F.,.F.,(4,1,1,1,1,1,
1,4),(53.4070751110265,53.856835863172,54.843296756577,55.829757649982,
56.816218543387,57.802679436792,58.789140330197,59.6902604182061),
 .UNSPECIFIED.);
#264=B_SPLINE_CURVE_WITH_KNOTS('',3,(#11256,#11257,#11258,#11259,#11260,
#11261,#11262,#11263,#11264,#11265,#11266),.UNSPECIFIED.,.F.,.F.,(4,1,1,
1,1,1,1,1,4),(47.1238898038469,47.3715810248879,48.3580419182929,49.3445028116979,
50.3309637051029,51.3174245985079,52.3038854919129,53.2903463853179,53.4070751110265),
 .UNSPECIFIED.);
#265=B_SPLINE_CURVE_WITH_KNOTS('',3,(#11267,#11268,#11269,#11270,#11271,
#11272,#11273,#11274,#11275,#11276),.UNSPECIFIED.,.F.,.F.,(4,1,1,1,1,1,
1,4),(47.1238898038469,47.9380705027419,48.9245313961469,49.9109922895519,
50.8974531829569,51.8839140763619,52.8703749697669,53.4070751110265),
 .UNSPECIFIED.);
#266=B_SPLINE_CURVE_WITH_KNOTS('',3,(#11281,#11282,#11283,#11284,#11285,
#11286,#11287,#11288,#11289,#11290),.UNSPECIFIED.,.F.,.F.,(4,1,1,1,1,1,
1,4),(40.8407044966673,41.4528156644579,42.4392765578629,43.4257374512679,
44.4121983446729,45.3986592380779,46.3851201314829,47.1238898038469),
 .UNSPECIFIED.);
#267=B_SPLINE_CURVE_WITH_KNOTS('',3,(#11291,#11292,#11293,#11294,#11295,
#11296,#11297,#11298,#11299,#11300,#11301),.UNSPECIFIED.,.F.,.F.,(4,1,1,
1,1,1,1,1,4),(40.8407044966673,41.0328442489069,42.0193051423119,43.0057660357169,
43.9922269291219,44.9786878225269,45.9651487159319,46.9516096093369,47.1238898038469),
 .UNSPECIFIED.);
#268=B_SPLINE_CURVE_WITH_KNOTS('',3,(#11306,#11307,#11308,#11309,#11310,
#11311,#11312,#11313,#11314,#11315),.UNSPECIFIED.,.F.,.F.,(4,1,1,1,1,1,
1,4),(34.5575191894877,35.5340503040279,36.5205111974329,37.5069720908379,
38.4934329842429,39.4798938776479,40.4663547710529,40.8407044966673),
 .UNSPECIFIED.);
#269=B_SPLINE_CURVE_WITH_KNOTS('',3,(#11316,#11317,#11318,#11319,#11320,
#11321,#11322,#11323,#11324,#11325),.UNSPECIFIED.,.F.,.F.,(4,1,1,1,1,1,
1,4),(34.5575191894877,35.1140788884769,36.1005397818819,37.0870006752869,
38.0734615686919,39.0599224620969,40.0463833555019,40.8407044966673),
 .UNSPECIFIED.);
#270=B_SPLINE_CURVE_WITH_KNOTS('',3,(#11330,#11331,#11332,#11333,#11334,
#11335,#11336,#11337,#11338,#11339,#11340),.UNSPECIFIED.,.F.,.F.,(4,1,1,
1,1,1,1,1,4),(28.2743338823081,28.6288240501929,29.6152849435979,30.6017458370029,
31.5882067304079,32.5746676238129,33.5611285172179,34.5475894106229,34.5575191894877),
 .UNSPECIFIED.);
#271=B_SPLINE_CURVE_WITH_KNOTS('',3,(#11341,#11342,#11343,#11344,#11345,
#11346,#11347,#11348,#11349,#11350),.UNSPECIFIED.,.F.,.F.,(4,1,1,1,1,1,
1,4),(28.2743338823081,29.1953135280469,30.1817744214519,31.1682353148569,
32.1546962082619,33.1411571016669,34.1276179950719,34.5575191894877),
 .UNSPECIFIED.);
#272=B_SPLINE_CURVE_WITH_KNOTS('',3,(#11355,#11356,#11357,#11358,#11359,
#11360,#11361,#11362,#11363,#11364),.UNSPECIFIED.,.F.,.F.,(4,1,1,1,1,1,
1,4),(21.9911485751285,22.7100586897628,23.6965195831678,24.6829804765729,
25.6694413699779,26.6559022633829,27.6423631567879,28.2743338823081),
 .UNSPECIFIED.);
#273=B_SPLINE_CURVE_WITH_KNOTS('',3,(#11365,#11366,#11367,#11368,#11369,
#11370,#11371,#11372,#11373,#11374,#11375),.UNSPECIFIED.,.F.,.F.,(4,1,1,
1,1,1,1,1,4),(21.9911485751285,22.2900872742119,23.2765481676169,24.2630090610219,
25.2494699544269,26.2359308478319,27.2223917412369,28.2088526346419,28.2743338823081),
 .UNSPECIFIED.);
#274=B_SPLINE_CURVE_WITH_KNOTS('',3,(#11381,#11382,#11383,#11384,#11385),
 .UNSPECIFIED.,.F.,.F.,(4,1,4),(14.3984001269718,15.3848610203768,15.7079632679489),
 .UNSPECIFIED.);
#275=B_SPLINE_CURVE_WITH_KNOTS('',3,(#11388,#11389,#11390,#11391,#11392),
 .UNSPECIFIED.,.F.,.F.,(4,1,4),(13.8759337553363,14.8183715425228,15.7079632679489),
 .UNSPECIFIED.);
#276=B_SPLINE_CURVE_WITH_KNOTS('',3,(#11436,#11437,#11438,#11439,#11440,
#11441,#11442,#11443,#11444,#11445,#11446),.UNSPECIFIED.,.F.,.F.,(4,1,1,
1,1,1,1,1,4),(15.7079632679489,15.8048324359278,16.7912933293328,17.7777542227378,
18.7642151161428,19.7506760095478,20.7371369029528,21.7235977963578,21.9911485751285),
 .UNSPECIFIED.);
#277=B_SPLINE_CURVE_WITH_KNOTS('',3,(#11447,#11448,#11449,#11450,#11451,
#11452,#11453,#11454,#11455,#11456),.UNSPECIFIED.,.F.,.F.,(4,1,1,1,1,1,
1,4),(15.7079632679489,16.3713219137818,17.3577828071869,18.3442437005919,
19.3307045939969,20.3171654874019,21.3036263808069,21.9911485751285),
 .UNSPECIFIED.);
#278=B_SPLINE_CURVE_WITH_KNOTS('',3,(#11681,#11682,#11683,#11684,#11685,
#11686,#11687,#11688,#11689,#11690,#11691,#11692,#11693,#11694,#11695,#11696,
#11697,#11698,#11699,#11700,#11701,#11702,#11703,#11704,#11705,#11706,#11707,
#11708,#11709,#11710,#11711,#11712,#11713,#11714,#11715,#11716,#11717,#11718,
#11719,#11720,#11721,#11722,#11723,#11724,#11725,#11726,#11727,#11728,#11729,
#11730,#11731,#11732,#11733,#11734,#11735,#11736,#11737,#11738),
 .UNSPECIFIED.,.F.,.F.,(4,3,3,3,3,3,3,3,3,3,3,3,3,3,3,3,3,3,3,4),(0.,0.0537021066009618,
0.0886282712367795,0.116609657471856,0.130919531620276,0.183454585359957,
0.216479690566366,0.230600805996023,0.244062534102707,0.292277144780104,
0.326690169730343,0.340044241140144,0.353800608199824,0.404857015795524,
0.431543783542484,0.447172905557772,0.495211581766649,0.520020647218237,
0.558026238582625,0.569248610399476),.UNSPECIFIED.);
#279=B_SPLINE_CURVE_WITH_KNOTS('',3,(#11739,#11740,#11741,#11742,#11743,
#11744,#11745,#11746,#11747,#11748,#11749,#11750,#11751,#11752,#11753,#11754,
#11755,#11756,#11757,#11758,#11759,#11760,#11761,#11762,#11763,#11764,#11765,
#11766,#11767,#11768,#11769,#11770,#11771,#11772,#11773,#11774,#11775,#11776,
#11777,#11778,#11779,#11780,#11781,#11782,#11783,#11784,#11785,#11786,#11787,
#11788,#11789,#11790,#11791,#11792,#11793,#11794,#11795,#11796),
 .UNSPECIFIED.,.F.,.F.,(4,3,3,3,3,3,3,3,3,3,3,3,3,3,3,3,3,3,3,4),(0.,0.0459570110526893,
0.0870590917386331,0.100825848951598,0.150050223978594,0.184086031790598,
0.203261017512761,0.21625650674859,0.263711469126828,0.302873338429799,
0.321032900850433,0.372046336254313,0.401845514967729,0.421231290172383,
0.435656368584207,0.474812416163248,0.492789265029642,0.5115498830849,0.553331205445793,
0.566847306048074),.UNSPECIFIED.);
#280=B_SPLINE_CURVE_WITH_KNOTS('',3,(#11797,#11798,#11799,#11800,#11801,
#11802,#11803,#11804,#11805,#11806,#11807,#11808,#11809,#11810,#11811,#11812,
#11813,#11814,#11815,#11816,#11817,#11818,#11819,#11820,#11821),
 .UNSPECIFIED.,.F.,.F.,(4,3,3,3,3,3,3,3,4),(-10.1321597128207,-9.86460893405003,
-8.87814804064502,-7.89168714724002,-6.90522625383502,-5.91876536043002,
-4.93230446702501,-3.94584357362001,-3.84897440564114),.UNSPECIFIED.);
#281=B_SPLINE_CURVE_WITH_KNOTS('',3,(#12046,#12047,#12048,#12049,#12050,
#12051,#12052,#12053,#12054,#12055,#12056,#12057,#12058,#12059,#12060,#12061,
#12062,#12063,#12064,#12065,#12066,#12067,#12068,#12069,#12070,#12071,#12072,
#12073,#12074,#12075,#12076,#12077,#12078,#12079,#12080,#12081,#12082,#12083,
#12084,#12085,#12086,#12087,#12088,#12089,#12090,#12091,#12092,#12093,#12094,
#12095,#12096,#12097,#12098,#12099,#12100,#12101,#12102,#12103),
 .UNSPECIFIED.,.F.,.F.,(4,3,3,3,3,3,3,3,3,3,3,3,3,3,3,3,3,3,3,4),(0.,0.0459569891390547,
0.0870591697117697,0.100825884142283,0.15005024998693,0.18408602471011,
0.203261079338359,0.216256514601739,0.263711469126829,0.302873340900277,
0.321032901451889,0.372046348770768,0.401845543858265,0.421231416110189,
0.435656634965766,0.474812764874804,0.492785320751935,0.511549417457807,
0.553331205445803,0.566847306048085),.UNSPECIFIED.);
#282=B_SPLINE_CURVE_WITH_KNOTS('',3,(#12104,#12105,#12106,#12107,#12108,
#12109,#12110,#12111,#12112,#12113,#12114,#12115,#12116,#12117,#12118,#12119,
#12120,#12121,#12122,#12123,#12124,#12125,#12126,#12127,#12128),
 .UNSPECIFIED.,.F.,.F.,(4,3,3,3,3,3,3,3,4),(7.59274844815668,7.89168714724002,
8.87814804064503,9.86460893405003,10.851069827455,11.83753072086,12.823991614265,
13.81045250767,13.8759337553363),.UNSPECIFIED.);
#283=B_SPLINE_CURVE_WITH_KNOTS('',3,(#12129,#12130,#12131,#12132,#12133,
#12134,#12135,#12136,#12137,#12138,#12139,#12140,#12141,#12142,#12143,#12144,
#12145,#12146,#12147,#12148,#12149,#12150,#12151,#12152,#12153,#12154,#12155,
#12156,#12157,#12158,#12159,#12160,#12161,#12162,#12163,#12164,#12165,#12166,
#12167,#12168,#12169,#12170,#12171,#12172,#12173,#12174,#12175,#12176,#12177,
#12178,#12179,#12180,#12181,#12182,#12183,#12184,#12185,#12186),
 .UNSPECIFIED.,.F.,.F.,(4,3,3,3,3,3,3,3,3,3,3,3,3,3,3,3,3,3,3,4),(0.,0.0537020933595249,
0.0886282312348469,0.116609505884768,0.130919504019768,0.183454564110696,
0.216479685514756,0.230600804284864,0.244062532276618,0.292277144780091,
0.326690174005652,0.34004425312577,0.353800612122922,0.404857018737847,
0.43154388809724,0.447172964606455,0.495211643185621,0.520020637237826,
0.558026238582621,0.569248610399474),.UNSPECIFIED.);
#284=B_SPLINE_CURVE_WITH_KNOTS('',3,(#12192,#12193,#12194,#12195,#12196,
#12197,#12198,#12199,#12200,#12201,#12202,#12203,#12204,#12205,#12206,#12207,
#12208,#12209,#12210,#12211,#12212,#12213,#12214,#12215,#12216,#12217,#12218,
#12219,#12220,#12221,#12222,#12223,#12224,#12225,#12226,#12227,#12228,#12229,
#12230,#12231,#12232,#12233,#12234,#12235,#12236,#12237,#12238,#12239,#12240,
#12241,#12242,#12243,#12244,#12245,#12246,#12247,#12248,#12249),
 .UNSPECIFIED.,.F.,.F.,(4,3,3,3,3,3,3,3,3,3,3,3,3,3,3,3,3,3,3,4),(0.,0.0459569597282421,
0.0870592743507417,0.100825931397392,0.150050284916509,0.184086015212499,
0.203261162306881,0.216256525140977,0.26371146912684,0.302873344212067,
0.321032902271426,0.372046365582263,0.401845582658033,0.421231585204367,
0.435656992651154,0.474813233102554,0.492780040699884,0.511548795880393,
0.553331205445832,0.566847306048113),.UNSPECIFIED.);
#285=B_SPLINE_CURVE_WITH_KNOTS('',3,(#12250,#12251,#12252,#12253,#12254,
#12255,#12256,#12257,#12258,#12259,#12260,#12261,#12262,#12263,#12264,#12265,
#12266,#12267,#12268,#12269,#12270,#12271,#12272,#12273,#12274,#12275,#12276,
#12277,#12278,#12279,#12280,#12281,#12282,#12283,#12284,#12285,#12286,#12287,
#12288,#12289,#12290,#12291,#12292,#12293,#12294,#12295,#12296,#12297,#12298,
#12299,#12300,#12301,#12302,#12303,#12304,#12305,#12306,#12307),
 .UNSPECIFIED.,.F.,.F.,(4,3,3,3,3,3,3,3,3,3,3,3,3,3,3,3,3,3,3,4),(0.,0.0537021278608587,
0.0886283354605565,0.116609900845683,0.130919575937586,0.183454619477383,
0.216479698675332,0.230600808889542,0.244062537057827,0.29227714478008,
0.326690162862484,0.340044221965521,0.353800601915901,0.404857011082572,
0.431543615670486,0.447172810805832,0.495211483201289,0.520020663253885,
0.558026238582585,0.569248610399439),.UNSPECIFIED.);
#286=B_SPLINE_CURVE_WITH_KNOTS('',3,(#12308,#12309,#12310,#12311,#12312,
#12313,#12314,#12315,#12316,#12317,#12318,#12319,#12320,#12321,#12322,#12323,
#12324,#12325,#12326,#12327,#12328,#12329,#12330,#12331,#12332,#12333,#12334,
#12335,#12336,#12337,#12338,#12339,#12340,#12341,#12342,#12343,#12344,#12345,
#12346,#12347,#12348,#12349,#12350,#12351,#12352,#12353,#12354,#12355,#12356,
#12357,#12358,#12359,#12360,#12361,#12362,#12363,#12364,#12365),
 .UNSPECIFIED.,.F.,.F.,(4,3,3,3,3,3,3,3,3,3,3,3,3,3,3,3,3,3,3,4),(0.,0.0459570233578969,
0.0870590479590349,0.100825829183884,0.150050209366866,0.184086035766608,
0.203260982741087,0.216256502330382,0.263711469126837,0.302873337041598,
0.321032900518168,0.372046329231869,0.40184549875999,0.421231219525568,
0.435656219182855,0.474812220578677,0.49279148193987,0.511550145279393,
0.553331205445819,0.566847306048101),.UNSPECIFIED.);
#287=B_SPLINE_CURVE_WITH_KNOTS('',3,(#12366,#12367,#12368,#12369,#12370,
#12371,#12372,#12373,#12374,#12375,#12376,#12377,#12378,#12379,#12380,#12381,
#12382,#12383,#12384,#12385,#12386,#12387,#12388,#12389,#12390,#12391,#12392,
#12393,#12394,#12395,#12396,#12397,#12398,#12399,#12400,#12401,#12402,#12403,
#12404,#12405,#12406,#12407,#12408,#12409,#12410,#12411,#12412,#12413,#12414,
#12415,#12416,#12417,#12418,#12419,#12420,#12421,#12422,#12423),
 .UNSPECIFIED.,.F.,.F.,(4,3,3,3,3,3,3,3,3,3,3,3,3,3,3,3,3,3,3,4),(0.,0.0537021066010595,
0.0886282712341201,0.116609657460836,0.130919531618635,0.18345458535817,
0.2164796905666,0.230600806130634,0.244062534124687,0.292277144780059,0.32669016973023,
0.340044241170799,0.35380060820706,0.40485701580094,0.431543783567626,0.447172905584617,
0.495211581792678,0.520020647237742,0.558026238582582,0.569248610399435),
 .UNSPECIFIED.);
#288=B_SPLINE_CURVE_WITH_KNOTS('',3,(#12424,#12425,#12426,#12427,#12428,
#12429,#12430,#12431,#12432,#12433,#12434,#12435,#12436,#12437,#12438,#12439,
#12440,#12441,#12442,#12443,#12444,#12445,#12446,#12447,#12448,#12449,#12450,
#12451,#12452,#12453,#12454,#12455,#12456,#12457,#12458,#12459,#12460,#12461,
#12462,#12463,#12464,#12465,#12466,#12467,#12468,#12469,#12470,#12471,#12472,
#12473,#12474,#12475,#12476,#12477,#12478,#12479,#12480,#12481),
 .UNSPECIFIED.,.F.,.F.,(4,3,3,3,3,3,3,3,3,3,3,3,3,3,3,3,3,3,3,4),(0.,0.0459569597282773,
0.0870592743559632,0.100825931391171,0.150050284910477,0.184086015212479,
0.203261162453712,0.216256525163335,0.263711469126836,0.302873344213503,
0.321032902268873,0.372046365578727,0.401845582651689,0.42123158516634,
0.435656992617324,0.474813233058503,0.492780041036963,0.511548795921555,
0.553331205445815,0.566847306048093),.UNSPECIFIED.);
#289=B_SPLINE_CURVE_WITH_KNOTS('',3,(#12482,#12483,#12484,#12485,#12486,
#12487,#12488,#12489,#12490,#12491,#12492,#12493,#12494,#12495,#12496,#12497,
#12498,#12499,#12500,#12501,#12502,#12503,#12504,#12505,#12506,#12507,#12508,
#12509,#12510,#12511,#12512,#12513,#12514,#12515,#12516,#12517,#12518,#12519,
#12520,#12521,#12522,#12523,#12524,#12525,#12526,#12527,#12528,#12529,#12530,
#12531,#12532,#12533,#12534,#12535,#12536,#12537,#12538,#12539),
 .UNSPECIFIED.,.F.,.F.,(4,3,3,3,3,3,3,3,3,3,3,3,3,3,3,3,3,3,3,4),(0.,0.0537021520206258,
0.0886284084442469,0.11661017742178,0.130919626307606,0.183454658252522,
0.216479707884859,0.230600812010997,0.244062540387362,0.292277144780059,
0.326690155053379,0.340044200114974,0.353800594757874,0.404857005714051,
0.43154342480673,0.447172703114038,0.495211371169167,0.520020681489528,
0.558026238582582,0.569248610399435),.UNSPECIFIED.);
#290=B_SPLINE_CURVE_WITH_KNOTS('',3,(#12541,#12542,#12543,#12544,#12545,
#12546,#12547,#12548,#12549,#12550,#12551),.UNSPECIFIED.,.F.,.F.,(4,1,1,
1,1,1,1,1,4),(15.7079632679489,15.8048324359278,16.7912933293328,17.7777542227378,
18.7642151161428,19.7506760095478,20.7371369029528,21.7235977963578,21.9911485751285),
 .UNSPECIFIED.);
#291=B_SPLINE_CURVE_WITH_KNOTS('',3,(#12552,#12553,#12554,#12555,#12556,
#12557,#12558,#12559,#12560,#12561),.UNSPECIFIED.,.F.,.F.,(4,1,1,1,1,1,
1,4),(15.7079632679489,16.3713219137818,17.3577828071869,18.3442437005919,
19.3307045939969,20.3171654874019,21.3036263808069,21.9911485751285),
 .UNSPECIFIED.);
#292=B_SPLINE_CURVE_WITH_KNOTS('',3,(#12786,#12787,#12788,#12789,#12790,
#12791,#12792,#12793,#12794,#12795,#12796,#12797,#12798,#12799,#12800,#12801,
#12802,#12803,#12804,#12805,#12806,#12807,#12808,#12809,#12810,#12811,#12812,
#12813,#12814,#12815,#12816,#12817,#12818,#12819,#12820,#12821,#12822,#12823,
#12824,#12825,#12826,#12827,#12828,#12829,#12830,#12831,#12832,#12833,#12834,
#12835,#12836,#12837,#12838,#12839,#12840,#12841,#12842,#12843),
 .UNSPECIFIED.,.F.,.F.,(4,3,3,3,3,3,3,3,3,3,3,3,3,3,3,3,3,3,3,4),(0.,0.0459570862230108,
0.087058824279425,0.100825728205661,0.150050134723767,0.184086056072108,
0.203260805225187,0.216256479777388,0.263711469126848,0.302873329947912,
0.321032898752379,0.372046293267176,0.401845415752178,0.421230857758822,
0.435655454101214,0.474811219031992,0.492802884326938,0.511551499405496,
0.553331205445843,0.566847306048125),.UNSPECIFIED.);
#293=B_SPLINE_CURVE_WITH_KNOTS('',3,(#12844,#12845,#12846,#12847,#12848,
#12849,#12850,#12851,#12852,#12853,#12854,#12855,#12856,#12857,#12858,#12859,
#12860,#12861,#12862,#12863,#12864,#12865,#12866,#12867,#12868),
 .UNSPECIFIED.,.F.,.F.,(4,3,3,3,3,3,3,3,4),(-10.1321597128207,-9.86460893405003,
-8.87814804064502,-7.89168714724002,-6.90522625383502,-5.91876536043002,
-4.93230446702501,-3.94584357362001,-3.84897440564114),.UNSPECIFIED.);
#294=B_SPLINE_CURVE_WITH_KNOTS('',3,(#13093,#13094,#13095,#13096,#13097,
#13098,#13099,#13100,#13101,#13102,#13103,#13104,#13105,#13106,#13107,#13108,
#13109,#13110,#13111,#13112,#13113,#13114,#13115,#13116,#13117),
 .UNSPECIFIED.,.F.,.F.,(4,3,3,3,3,3,3,3,4),(7.59274844815667,7.89168714724002,
8.87814804064503,9.86460893405003,10.851069827455,11.83753072086,12.823991614265,
13.81045250767,13.8759337553363),.UNSPECIFIED.);
#295=B_SPLINE_CURVE_WITH_KNOTS('',3,(#13118,#13119,#13120,#13121,#13122,
#13123,#13124,#13125,#13126,#13127,#13128,#13129,#13130,#13131,#13132,#13133,
#13134,#13135,#13136,#13137,#13138,#13139,#13140,#13141,#13142,#13143,#13144,
#13145,#13146,#13147,#13148,#13149,#13150,#13151,#13152,#13153,#13154,#13155,
#13156,#13157,#13158,#13159,#13160,#13161,#13162,#13163,#13164,#13165,#13166,
#13167,#13168,#13169,#13170,#13171,#13172,#13173,#13174,#13175),
 .UNSPECIFIED.,.F.,.F.,(4,3,3,3,3,3,3,3,3,3,3,3,3,3,3,3,3,3,3,4),(0.,0.0537020755871833,
0.0886281775480827,0.116609302441915,0.130919466980084,0.183454535593745,
0.216479678733881,0.230600801897488,0.244062529810022,0.292277144780066,
0.326690179741516,0.340044269166468,0.353800617376193,0.404857022677782,
0.431544028354177,0.447173043816862,0.495211725573931,0.52002062383812,
0.558026238582546,0.569248610399397),.UNSPECIFIED.);
#296=B_SPLINE_CURVE_WITH_KNOTS('',3,(#13177,#13178,#13179,#13180,#13181,
#13182,#13183,#13184,#13185,#13186,#13187),.UNSPECIFIED.,.F.,.F.,(4,1,1,
1,1,1,1,1,4),(15.7079632679489,15.8048324359278,16.7912933293328,17.7777542227378,
18.7642151161428,19.7506760095478,20.7371369029528,21.7235977963578,21.9911485751285),
 .UNSPECIFIED.);
#297=B_SPLINE_CURVE_WITH_KNOTS('',3,(#13188,#13189,#13190,#13191,#13192,
#13193,#13194,#13195,#13196,#13197),.UNSPECIFIED.,.F.,.F.,(4,1,1,1,1,1,
1,4),(15.7079632679489,16.3713219137818,17.3577828071869,18.3442437005919,
19.3307045939969,20.3171654874019,21.3036263808069,21.9911485751285),
 .UNSPECIFIED.);
#298=B_SPLINE_CURVE_WITH_KNOTS('',3,(#13422,#13423,#13424,#13425,#13426,
#13427,#13428,#13429,#13430,#13431,#13432,#13433,#13434,#13435,#13436,#13437,
#13438,#13439,#13440,#13441,#13442,#13443,#13444,#13445,#13446,#13447,#13448,
#13449,#13450,#13451,#13452,#13453,#13454,#13455,#13456,#13457,#13458,#13459,
#13460,#13461,#13462,#13463,#13464,#13465,#13466,#13467,#13468,#13469,#13470,
#13471,#13472,#13473,#13474,#13475,#13476,#13477,#13478,#13479),
 .UNSPECIFIED.,.F.,.F.,(4,3,3,3,3,3,3,3,3,3,3,3,3,3,3,3,3,3,3,4),(0.,0.0459570110528117,
0.0870590917382537,0.100825848948781,0.150050223975658,0.18408603179036,
0.203261017504252,0.216256506747385,0.263711469126848,0.302873338429924,
0.3210329008499,0.37204633625366,0.401845514966252,0.421231290165854,0.435656368582237,
0.47481241616036,0.492789265129085,0.511549883096662,0.553331205445843,
0.566847306048125),.UNSPECIFIED.);
#299=B_SPLINE_CURVE_WITH_KNOTS('',3,(#13480,#13481,#13482,#13483,#13484,
#13485,#13486,#13487,#13488,#13489,#13490,#13491,#13492,#13493,#13494,#13495,
#13496,#13497,#13498,#13499,#13500,#13501,#13502,#13503,#13504),
 .UNSPECIFIED.,.F.,.F.,(4,3,3,3,3,3,3,3,4),(-10.1321597128207,-9.86460893405003,
-8.87814804064502,-7.89168714724002,-6.90522625383502,-5.91876536043002,
-4.93230446702501,-3.94584357362001,-3.84897440564114),.UNSPECIFIED.);
#300=B_SPLINE_CURVE_WITH_KNOTS('',3,(#13729,#13730,#13731,#13732,#13733,
#13734,#13735,#13736,#13737,#13738,#13739,#13740,#13741,#13742,#13743,#13744,
#13745,#13746,#13747,#13748,#13749,#13750,#13751,#13752,#13753),
 .UNSPECIFIED.,.F.,.F.,(4,3,3,3,3,3,3,3,4),(7.59274844815667,7.89168714724002,
8.87814804064503,9.86460893405003,10.851069827455,11.83753072086,12.823991614265,
13.81045250767,13.8759337553363),.UNSPECIFIED.);
#301=B_SPLINE_CURVE_WITH_KNOTS('',3,(#13754,#13755,#13756,#13757,#13758,
#13759,#13760,#13761,#13762,#13763,#13764,#13765,#13766,#13767,#13768,#13769,
#13770,#13771,#13772,#13773,#13774,#13775,#13776,#13777,#13778,#13779,#13780,
#13781,#13782,#13783,#13784,#13785,#13786,#13787,#13788,#13789,#13790,#13791,
#13792,#13793,#13794,#13795,#13796,#13797,#13798,#13799,#13800,#13801,#13802,
#13803,#13804,#13805,#13806,#13807,#13808,#13809,#13810,#13811),
 .UNSPECIFIED.,.F.,.F.,(4,3,3,3,3,3,3,3,3,3,3,3,3,3,3,3,3,3,3,4),(0.,0.053702114036519,
0.0886282936969937,0.116609742583596,0.130919547118421,0.18345459729122,
0.216479693402787,0.230600807019328,0.244062535138244,0.292277144780066,
0.326690167328717,0.340044234449132,0.353800606005677,0.404857014149894,
0.431543724850428,0.447172872441803,0.495211547318113,0.520020652828403,
0.558026238582546,0.569248610399397),.UNSPECIFIED.);
#302=B_SPLINE_CURVE_WITH_KNOTS('',3,(#13813,#13814,#13815,#13816,#13817,
#13818,#13819,#13820,#13821,#13822,#13823),.UNSPECIFIED.,.F.,.F.,(4,1,1,
1,1,1,1,1,4),(15.7079632679489,15.8048324359278,16.7912933293328,17.7777542227378,
18.7642151161428,19.7506760095478,20.7371369029528,21.7235977963578,21.9911485751285),
 .UNSPECIFIED.);
#303=B_SPLINE_CURVE_WITH_KNOTS('',3,(#13824,#13825,#13826,#13827,#13828,
#13829,#13830,#13831,#13832,#13833),.UNSPECIFIED.,.F.,.F.,(4,1,1,1,1,1,
1,4),(15.7079632679489,16.3713219137818,17.3577828071869,18.3442437005919,
19.3307045939969,20.3171654874019,21.3036263808069,21.9911485751285),
 .UNSPECIFIED.);
#304=B_SPLINE_CURVE_WITH_KNOTS('',3,(#14058,#14059,#14060,#14061,#14062,
#14063,#14064,#14065,#14066,#14067,#14068,#14069,#14070,#14071,#14072,#14073,
#14074,#14075,#14076,#14077,#14078,#14079,#14080,#14081,#14082,#14083,#14084,
#14085,#14086,#14087,#14088,#14089,#14090,#14091,#14092,#14093,#14094,#14095,
#14096,#14097,#14098,#14099,#14100,#14101,#14102,#14103,#14104,#14105,#14106,
#14107,#14108,#14109,#14110,#14111,#14112,#14113,#14114,#14115),
 .UNSPECIFIED.,.F.,.F.,(4,3,3,3,3,3,3,3,3,3,3,3,3,3,3,3,3,3,3,4),(0.,0.0459570462372587,
0.0870589665518601,0.100825792431561,0.150050182199626,0.184086043156091,
0.203260918169112,0.216256494127592,0.263711469126833,0.302873334461669,
0.321032899868711,0.372046316136279,0.401845468535358,0.421231087805859,
0.435655940588184,0.474811855885159,0.492795623998078,0.511550636110964,
0.553331205445823,0.566847306048107),.UNSPECIFIED.);
#305=B_SPLINE_CURVE_WITH_KNOTS('',3,(#14116,#14117,#14118,#14119,#14120,
#14121,#14122,#14123,#14124,#14125,#14126,#14127,#14128,#14129,#14130,#14131,
#14132,#14133,#14134,#14135,#14136,#14137,#14138,#14139,#14140),
 .UNSPECIFIED.,.F.,.F.,(4,3,3,3,3,3,3,3,4),(-10.1321597128207,-9.86460893405003,
-8.87814804064502,-7.89168714724003,-6.90522625383502,-5.91876536043002,
-4.93230446702501,-3.94584357362001,-3.84897440564113),.UNSPECIFIED.);
#306=B_SPLINE_CURVE_WITH_KNOTS('',3,(#14365,#14366,#14367,#14368,#14369,
#14370,#14371,#14372,#14373,#14374,#14375,#14376,#14377,#14378,#14379,#14380,
#14381,#14382,#14383,#14384,#14385,#14386,#14387,#14388,#14389),
 .UNSPECIFIED.,.F.,.F.,(4,3,3,3,3,3,3,3,4),(7.59274844815667,7.89168714724002,
8.87814804064502,9.86460893405003,10.851069827455,11.83753072086,12.823991614265,
13.81045250767,13.8759337553363),.UNSPECIFIED.);
#307=B_SPLINE_CURVE_WITH_KNOTS('',3,(#14390,#14391,#14392,#14393,#14394,
#14395,#14396,#14397,#14398,#14399,#14400,#14401,#14402,#14403,#14404,#14405,
#14406,#14407,#14408,#14409,#14410,#14411,#14412,#14413,#14414,#14415,#14416,
#14417,#14418,#14419,#14420,#14421,#14422,#14423,#14424,#14425,#14426,#14427,
#14428,#14429,#14430,#14431,#14432,#14433,#14434,#14435,#14436,#14437,#14438,
#14439,#14440,#14441,#14442,#14443,#14444,#14445,#14446,#14447),
 .UNSPECIFIED.,.F.,.F.,(4,3,3,3,3,3,3,3,3,3,3,3,3,3,3,3,3,3,3,4),(0.,0.0537020755872334,
0.088628177548111,0.116609302442254,0.130919466980116,0.183454535593798,
0.216479678733695,0.230600801901911,0.244062529810737,0.292277144780056,
0.326690179741613,0.340044269176976,0.353800617378764,0.40485702267971,
0.431544028358992,0.447173043821804,0.495211725577524,0.520020623835711,
0.558026238582547,0.5692486103994),.UNSPECIFIED.);
#308=B_SPLINE_CURVE_WITH_KNOTS('',3,(#14682,#14683,#14684,#14685,#14686,
#14687,#14688,#14689,#14690,#14691,#14692,#14693,#14694,#14695,#14696,#14697,
#14698,#14699),.UNSPECIFIED.,.F.,.F.,(4,2,2,2,2,2,2,2,4),(0.,0.340227238436096,
0.680454476872192,1.02068171530829,1.36090895374438,1.70110830750183,2.04130766125928,
2.38150701501673,2.72170636877417),.UNSPECIFIED.);
#309=B_SPLINE_CURVE_WITH_KNOTS('',3,(#14700,#14701,#14702,#14703,#14704,
#14705,#14706,#14707,#14708,#14709,#14710,#14711,#14712,#14713,#14714,#14715,
#14716,#14717,#14718,#14719,#14720,#14721,#14722,#14723,#14724,#14725,#14726,
#14727,#14728,#14729,#14730,#14731,#14732,#14733,#14734,#14735,#14736,#14737,
#14738,#14739,#14740,#14741,#14742,#14743,#14744,#14745,#14746,#14747,#14748,
#14749),.UNSPECIFIED.,.F.,.F.,(4,2,2,2,2,2,2,2,2,2,2,2,2,2,2,2,2,2,2,2,
2,2,2,2,4),(2.72170636877417,3.06190572253162,3.40210507628907,3.74230443004652,
4.08250378380397,4.42273102224006,4.76295826067616,5.10318549911225,5.44341273754835,
5.78363997598445,6.12386721442054,6.46409445285664,6.80432169129273,7.14452104505018,
7.48472039880763,7.82491975256507,8.16511910632252,8.50531846007997,8.84551781383742,
9.18571716759487,9.52591652135231,9.86614375978841,10.2063709982245,10.5465982366606,
10.8868254750967),.UNSPECIFIED.);
#310=B_SPLINE_CURVE_WITH_KNOTS('',3,(#14755,#14756,#14757,#14758,#14759,
#14760,#14761,#14762,#14763,#14764,#14765,#14766,#14767,#14768,#14769,#14770,
#14771,#14772,#14773,#14774,#14775,#14776,#14777,#14778,#14779,#14780,#14781,
#14782,#14783,#14784,#14785,#14786,#14787,#14788,#14789,#14790,#14791,#14792,
#14793,#14794,#14795,#14796,#14797,#14798,#14799,#14800,#14801,#14802,#14803,
#14804,#14805,#14806,#14807,#14808,#14809),.UNSPECIFIED.,.F.,.F.,(4,2,2,
2,2,2,2,2,2,2,2,2,2,2,2,2,2,2,2,2,2,3,2,2,2,2,4),(-7.01225091221826,-6.82312918521928,
-6.48193726869111,-6.14074535216294,-5.79955343563477,-5.4583615191066,
-5.11716960257843,-4.77597768605026,-4.43478576952209,-4.09359385299392,
-3.75249057963376,-3.41138730627361,-3.07028403291345,-2.7291807595533,
-2.38807748619315,-2.04697421283299,-1.70587093947284,-1.36476766611268,
-1.02357574958451,-0.68238383305634,-0.341191916528169,0.,0.34119191652817,
0.68238383305634,1.02357574958451,1.36476766611268,1.55388939311326),
 .UNSPECIFIED.);
#311=B_SPLINE_CURVE_WITH_KNOTS('',3,(#14886,#14887,#14888,#14889,#14890,
#14891,#14892,#14893,#14894,#14895),.UNSPECIFIED.,.F.,.F.,(4,2,2,2,4),(-0.455064911568752,
-0.341315631981151,-0.227566352393549,-0.113783176196775,0.),
 .UNSPECIFIED.);
#312=B_SPLINE_CURVE_WITH_KNOTS('',3,(#14898,#14899,#14900,#14901,#14902,
#14903,#14904,#14905,#14906,#14907),.UNSPECIFIED.,.F.,.F.,(4,2,2,2,4),(-0.910129823137504,
-0.796346646940729,-0.682563470743954,-0.568814191156353,-0.455064911568752),
 .UNSPECIFIED.);
#313=B_SPLINE_CURVE_WITH_KNOTS('',3,(#14920,#14921,#14922,#14923,#14924,
#14925,#14926,#14927,#14928,#14929,#14930,#14931,#14932,#14933,#14934,#14935,
#14936,#14937),.UNSPECIFIED.,.F.,.F.,(4,2,2,2,2,2,2,2,4),(0.,0.113783176196775,
0.227566352393549,0.34131563198115,0.455064911568751,0.568814191156352,
0.682563470743952,0.796346646940728,0.910129823137503),.UNSPECIFIED.);
#314=B_SPLINE_CURVE_WITH_KNOTS('',3,(#14963,#14964,#14965,#14966,#14967,
#14968,#14969,#14970,#14971,#14972,#14973,#14974,#14975,#14976,#14977,#14978,
#14979,#14980),.UNSPECIFIED.,.F.,.F.,(4,2,2,2,2,2,2,2,4),(-0.910129823137502,
-0.796346646940727,-0.682563470743952,-0.568814191156352,-0.455064911568751,
-0.34131563198115,-0.227566352393549,-0.113783176196775,0.),
 .UNSPECIFIED.);
#315=B_SPLINE_CURVE_WITH_KNOTS('',3,(#14991,#14992,#14993,#14994,#14995,
#14996,#14997,#14998,#14999,#15000,#15001,#15002,#15003,#15004,#15005,#15006,
#15007,#15008),.UNSPECIFIED.,.F.,.F.,(4,2,2,2,2,2,2,2,4),(0.,0.113783176196775,
0.227566352393549,0.34131563198115,0.455064911568751,0.568814191156351,
0.682563470743952,0.796346646940727,0.910129823137502),.UNSPECIFIED.);
#316=B_SPLINE_CURVE_WITH_KNOTS('',3,(#15022,#15023,#15024,#15025,#15026,
#15027,#15028,#15029,#15030,#15031,#15032,#15033,#15034,#15035,#15036,#15037,
#15038,#15039),.UNSPECIFIED.,.F.,.F.,(4,2,2,2,2,2,2,2,4),(-0.910129823137502,
-0.796346646940727,-0.682563470743952,-0.568814191156352,-0.455064911568751,
-0.34131563198115,-0.22756635239355,-0.113783176196775,0.),
 .UNSPECIFIED.);
#317=B_SPLINE_CURVE_WITH_KNOTS('',3,(#15050,#15051,#15052,#15053,#15054,
#15055,#15056,#15057,#15058,#15059,#15060,#15061,#15062,#15063,#15064,#15065,
#15066,#15067),.UNSPECIFIED.,.F.,.F.,(4,2,2,2,2,2,2,2,4),(0.,0.113783176196775,
0.22756635239355,0.341315631981151,0.455064911568751,0.568814191156352,
0.682563470743953,0.796346646940727,0.910129823137502),.UNSPECIFIED.);
#318=B_SPLINE_CURVE_WITH_KNOTS('',3,(#15280,#15281,#15282,#15283,#15284,
#15285,#15286,#15287,#15288,#15289),.UNSPECIFIED.,.F.,.F.,(4,3,3,4),(-4.09293042013064,
-3.99414235995773,-2.99560676996829,-2.0686381749092),.UNSPECIFIED.);
#319=B_SPLINE_CURVE_WITH_KNOTS('',3,(#15297,#15298,#15299,#15300,#15301,
#15302,#15303),.UNSPECIFIED.,.F.,.F.,(4,3,4),(0.,0.999966929888035,1.11730040836829),
 .UNSPECIFIED.);
#320=B_SPLINE_CURVE_WITH_KNOTS('',3,(#15308,#15309,#15310,#15311,#15312,
#15313,#15314,#15315,#15316,#15317,#15318,#15319,#15320,#15321,#15322,#15323,
#15324,#15325,#15326,#15327,#15328,#15329),.UNSPECIFIED.,.F.,.F.,(4,3,3,
3,3,3,3,4),(-10.3761157273102,-9.98535589989431,-8.98682030990488,-7.98828471991545,
-6.98974912992602,-5.99121353993659,-4.99267794994716,-4.09293042013064),
 .UNSPECIFIED.);
#321=B_SPLINE_CURVE_WITH_KNOTS('',3,(#15330,#15331,#15332,#15333,#15334,
#15335,#15336,#15337,#15338,#15339,#15340,#15341,#15342,#15343,#15344,#15345,
#15346,#15347,#15348,#15349,#15350,#15351),.UNSPECIFIED.,.F.,.F.,(4,3,3,
3,3,3,3,4),(1.11730040836829,1.99993385977607,2.99990078966411,3.99986771955214,
4.99983464944018,5.99980157932822,6.99976850921625,7.40048571554796),
 .UNSPECIFIED.);
#322=B_SPLINE_CURVE_WITH_KNOTS('',3,(#15356,#15357,#15358,#15359,#15360,
#15361,#15362,#15363,#15364,#15365,#15366,#15367,#15368,#15369,#15370,#15371,
#15372,#15373,#15374,#15375,#15376,#15377),.UNSPECIFIED.,.F.,.F.,(4,3,3,
3,3,3,3,4),(-16.6593010344898,-15.9765694398309,-14.9780338498415,-13.979498259852,
-12.9809626698626,-11.9824270798732,-10.9838914898837,-10.3761157273102),
 .UNSPECIFIED.);
#323=B_SPLINE_CURVE_WITH_KNOTS('',3,(#15378,#15379,#15380,#15381,#15382,
#15383,#15384,#15385,#15386,#15387,#15388,#15389,#15390,#15391,#15392,#15393,
#15394,#15395,#15396,#15397,#15398,#15399),.UNSPECIFIED.,.F.,.F.,(4,3,3,
3,3,3,3,4),(7.40048571554796,7.99973543910429,8.99970236899232,9.99966929888036,
10.9996362287684,11.9996031586564,12.9995700885445,13.6836710227275),
 .UNSPECIFIED.);
#324=B_SPLINE_CURVE_WITH_KNOTS('',3,(#15404,#15405,#15406,#15407,#15408,
#15409,#15410,#15411,#15412,#15413,#15414,#15415,#15416,#15417,#15418,#15419,
#15420,#15421,#15422,#15423,#15424,#15425),.UNSPECIFIED.,.F.,.F.,(4,3,3,
3,3,3,3,4),(-22.9424863416693,-21.9677829797675,-20.9692473897781,-19.9707117997886,
-18.9721762097992,-17.9736406198098,-16.9751050298203,-16.6593010344898),
 .UNSPECIFIED.);
#325=B_SPLINE_CURVE_WITH_KNOTS('',3,(#15426,#15427,#15428,#15429,#15430,
#15431,#15432,#15433,#15434,#15435,#15436,#15437,#15438,#15439,#15440,#15441,
#15442,#15443,#15444,#15445,#15446,#15447),.UNSPECIFIED.,.F.,.F.,(4,3,3,
3,3,3,3,4),(13.6836710227275,13.9995370184325,14.9995039483205,15.9994708782086,
16.9994378080966,17.9994047379846,18.9993716678727,19.9668563299071),
 .UNSPECIFIED.);
#326=B_SPLINE_CURVE_WITH_KNOTS('',3,(#15452,#15453,#15454,#15455,#15456,
#15457,#15458,#15459,#15460,#15461,#15462,#15463,#15464,#15465,#15466,#15467,
#15468,#15469,#15470,#15471,#15472,#15473,#15474,#15475,#15476),
 .UNSPECIFIED.,.F.,.F.,(4,3,3,3,3,3,3,3,4),(-29.225671648849,-28.9575321096935,
-27.9589965197041,-26.9604609297146,-25.9619253397252,-24.9633897497358,
-23.9648541597464,-22.9663185697569,-22.9424863416693),.UNSPECIFIED.);
#327=B_SPLINE_CURVE_WITH_KNOTS('',3,(#15477,#15478,#15479,#15480,#15481,
#15482,#15483,#15484,#15485,#15486,#15487,#15488,#15489,#15490,#15491,#15492,
#15493,#15494,#15495,#15496,#15497,#15498,#15499,#15500,#15501),
 .UNSPECIFIED.,.F.,.F.,(4,3,3,3,3,3,3,3,4),(19.9668563299071,19.9993385977607,
20.9993055276488,21.9992724575368,22.9992393874248,23.9992063173129,24.9991732472009,
25.9991401770889,26.2500416370867),.UNSPECIFIED.);
#328=B_SPLINE_CURVE_WITH_KNOTS('',3,(#15506,#15507,#15508,#15509,#15510,
#15511,#15512,#15513,#15514,#15515,#15516,#15517,#15518,#15519,#15520,#15521,
#15522,#15523,#15524,#15525,#15526,#15527),.UNSPECIFIED.,.F.,.F.,(4,3,3,
3,3,3,3,4),(-35.5088569560286,-34.9487456496301,-33.9502100596407,-32.9516744696512,
-31.9531388796618,-30.9546032896724,-29.9560676996829,-29.225671648849),
 .UNSPECIFIED.);
#329=B_SPLINE_CURVE_WITH_KNOTS('',3,(#15528,#15529,#15530,#15531,#15532,
#15533,#15534,#15535,#15536,#15537,#15538,#15539,#15540,#15541,#15542,#15543,
#15544,#15545,#15546,#15547,#15548,#15549),.UNSPECIFIED.,.F.,.F.,(4,3,3,
3,3,3,3,4),(26.2500416370867,26.999107106977,27.999074036865,28.999040966753,
29.9990078966411,30.9989748265291,31.9989417564172,32.5332269442662),
 .UNSPECIFIED.);
#330=B_SPLINE_CURVE_WITH_KNOTS('',3,(#15554,#15555,#15556,#15557,#15558,
#15559,#15560,#15561,#15562,#15563,#15564,#15565,#15566,#15567,#15568,#15569,
#15570,#15571,#15572,#15573,#15574,#15575),.UNSPECIFIED.,.F.,.F.,(4,3,3,
3,3,3,3,4),(-41.7920422632081,-40.9399591895667,-39.9414235995773,-38.9428880095878,
-37.9443524195984,-36.945816829609,-35.9472812396195,-35.5088569560286),
 .UNSPECIFIED.);
#331=B_SPLINE_CURVE_WITH_KNOTS('',3,(#15576,#15577,#15578,#15579,#15580,
#15581,#15582,#15583,#15584,#15585,#15586,#15587,#15588,#15589,#15590,#15591,
#15592,#15593,#15594,#15595,#15596,#15597),.UNSPECIFIED.,.F.,.F.,(4,3,3,
3,3,3,3,4),(32.5332269442662,32.9989086863052,33.9988756161932,34.9988425460813,
35.9988094759693,36.9987764058573,37.9987433357454,38.8164122514459),
 .UNSPECIFIED.);
#332=B_SPLINE_CURVE_WITH_KNOTS('',3,(#15603,#15604,#15605,#15606,#15607,
#15608,#15609,#15610,#15611,#15612),.UNSPECIFIED.,.F.,.F.,(4,1,1,1,1,1,
1,4),(53.4070751110265,53.5535276273744,54.5520632173639,55.5505988073533,
56.5491343973427,57.5476699873322,58.5462055773216,59.544741167311),
 .UNSPECIFIED.);
#333=B_SPLINE_CURVE_WITH_KNOTS('',3,(#15615,#15616,#15617,#15618,#15619,
#15620,#15621,#15622),.UNSPECIFIED.,.F.,.F.,(4,1,1,1,1,4),(53.4070751110265,
54.3059563272507,55.3059232571387,56.3058901870267,57.3058571169148,58.3058240468028),
 .UNSPECIFIED.);
#334=B_SPLINE_CURVE_WITH_KNOTS('',3,(#15627,#15628,#15629,#15630,#15631,
#15632,#15633,#15634,#15635,#15636),.UNSPECIFIED.,.F.,.F.,(4,1,1,1,1,1,
1,4),(47.1238898038469,47.5623140874379,48.5608496774273,49.5593852674167,
50.5579208574061,51.5564564473956,52.554992037385,53.4070751110265),
 .UNSPECIFIED.);
#335=B_SPLINE_CURVE_WITH_KNOTS('',3,(#15637,#15638,#15639,#15640,#15641,
#15642,#15643,#15644,#15645,#15646,#15647),.UNSPECIFIED.,.F.,.F.,(4,1,1,
1,1,1,1,1,4),(47.1238898038469,47.3061878180344,48.3061547479224,49.3061216778105,
50.3060886076985,51.3060555375865,52.3060224674746,53.3059893973626,53.4070751110265),
 .UNSPECIFIED.);
#336=B_SPLINE_CURVE_WITH_KNOTS('',3,(#15652,#15653,#15654,#15655,#15656,
#15657,#15658,#15659,#15660,#15661),.UNSPECIFIED.,.F.,.F.,(4,1,1,1,1,1,
1,4),(40.8407044966673,41.5711005475013,42.5696361374907,43.5681717274801,
44.5667073174696,45.565242907459,46.5637784974484,47.1238898038469),
 .UNSPECIFIED.);
#337=B_SPLINE_CURVE_WITH_KNOTS('',3,(#15662,#15663,#15664,#15665,#15666,
#15667,#15668,#15669,#15670,#15671),.UNSPECIFIED.,.F.,.F.,(4,1,1,1,1,1,
1,4),(40.8407044966673,41.3063862387062,42.3063531685942,43.3063200984823,
44.3062870283703,45.3062539582583,46.3062208881464,47.1238898038469),
 .UNSPECIFIED.);
#338=B_SPLINE_CURVE_WITH_KNOTS('',3,(#15676,#15677,#15678,#15679,#15680,
#15681,#15682,#15683,#15684,#15685,#15686),.UNSPECIFIED.,.F.,.F.,(4,1,1,
1,1,1,1,1,4),(34.5575191894877,34.5813514175752,35.5798870075647,36.5784225975541,
37.5769581875435,38.575493777533,39.5740293675224,40.5725649575118,40.8407044966673),
 .UNSPECIFIED.);
#339=B_SPLINE_CURVE_WITH_KNOTS('',3,(#15687,#15688,#15689,#15690,#15691,
#15692,#15693,#15694,#15695,#15696),.UNSPECIFIED.,.F.,.F.,(4,1,1,1,1,1,
1,4),(34.5575191894877,35.306584659378,36.306551589266,37.306518519154,
38.3064854490421,39.3064523789301,40.3064193088181,40.8407044966673),
 .UNSPECIFIED.);
#340=B_SPLINE_CURVE_WITH_KNOTS('',3,(#15701,#15702,#15703,#15704,#15705,
#15706,#15707,#15708,#15709,#15710),.UNSPECIFIED.,.F.,.F.,(4,1,1,1,1,1,
1,4),(28.2743338823081,28.5901378776387,29.5886734676281,30.5872090576175,
31.585744647607,32.5842802375964,33.5828158275858,34.5575191894877),
 .UNSPECIFIED.);
#341=B_SPLINE_CURVE_WITH_KNOTS('',3,(#15711,#15712,#15713,#15714,#15715,
#15716,#15717,#15718,#15719,#15720,#15721),.UNSPECIFIED.,.F.,.F.,(4,1,1,
1,1,1,1,1,4),(28.2743338823081,28.3068161501617,29.3067830800498,30.3067500099378,
31.3067169398258,32.3066838697139,33.3066507996019,34.3066177294899,34.5575191894877),
 .UNSPECIFIED.);
#342=B_SPLINE_CURVE_WITH_KNOTS('',3,(#15726,#15727,#15728,#15729,#15730,
#15731,#15732,#15733,#15734,#15735),.UNSPECIFIED.,.F.,.F.,(4,1,1,1,1,1,
1,4),(21.9911485751285,22.5989243377021,23.5974599276915,24.5959955176809,
25.5945311076704,26.5930666976598,27.5916022876492,28.2743338823081),
 .UNSPECIFIED.);
#343=B_SPLINE_CURVE_WITH_KNOTS('',3,(#15736,#15737,#15738,#15739,#15740,
#15741,#15742,#15743,#15744,#15745),.UNSPECIFIED.,.F.,.F.,(4,1,1,1,1,1,
1,4),(21.9911485751285,22.3070145708335,23.3069815007215,24.3069484306096,
25.3069153604976,26.3068822903856,27.3068492202737,28.2743338823081),
 .UNSPECIFIED.);
#344=B_SPLINE_CURVE_WITH_KNOTS('',3,(#15750,#15751,#15752,#15753,#15754,
#15755,#15756,#15757,#15758,#15759),.UNSPECIFIED.,.F.,.F.,(4,1,1,1,1,1,
1,4),(15.707963267949,16.6077107977655,17.6062463877549,18.6047819777443,
19.6033175677338,20.6018531577232,21.6003887477126,21.9911485751285),
 .UNSPECIFIED.);
#345=B_SPLINE_CURVE_WITH_KNOTS('',3,(#15760,#15761,#15762,#15763,#15764,
#15765,#15766,#15767,#15768,#15769),.UNSPECIFIED.,.F.,.F.,(4,1,1,1,1,1,
1,4),(15.707963267949,16.3072129915053,17.3071799213933,18.3071468512814,
19.3071137811694,20.3070807110574,21.3070476409455,21.9911485751285),
 .UNSPECIFIED.);
#346=B_SPLINE_CURVE_WITH_KNOTS('',3,(#15772,#15773,#15774,#15775,#15776,
#15777,#15778,#15779,#15780,#15781,#15782,#15783,#15784,#15785,#15786,#15787,
#15788,#15789,#15790,#15791,#15792,#15793,#15794,#15795,#15796,#15797,#15798,
#15799,#15800,#15801,#15802,#15803,#15804,#15805,#15806,#15807,#15808,#15809,
#15810,#15811,#15812,#15813,#15814,#15815,#15816,#15817,#15818,#15819,#15820,
#15821,#15822,#15823,#15824,#15825,#15826,#15827,#15828,#15829,#15830,#15831,
#15832,#15833,#15834,#15835,#15836,#15837,#15838,#15839,#15840,#15841,#15842,
#15843,#15844,#15845,#15846,#15847,#15848,#15849,#15850,#15851,#15852,#15853,
#15854,#15855,#15856,#15857,#15858,#15859,#15860,#15861,#15862,#15863,#15864,
#15865,#15866,#15867,#15868,#15869,#15870,#15871,#15872,#15873,#15874,#15875,
#15876,#15877,#15878,#15879,#15880,#15881,#15882,#15883,#15884,#15885,#15886,
#15887,#15888,#15889,#15890,#15891,#15892,#15893,#15894,#15895,#15896,#15897,
#15898,#15899,#15900,#15901,#15902,#15903,#15904,#15905,#15906,#15907,#15908,
#15909,#15910),.UNSPECIFIED.,.F.,.F.,(4,3,3,3,3,3,3,3,3,3,3,3,3,3,3,3,3,
3,3,3,3,3,3,3,3,3,3,3,3,3,3,3,3,3,3,3,3,3,3,3,3,3,3,3,3,3,4),(-1.51155304937198,
-1.46675125746741,-1.44534760943282,-1.43064097934658,-1.38981975448008,
-1.37050017754913,-1.35786409561476,-1.31261008774766,-1.28845427025889,
-1.27348742951611,-1.26735607988056,-1.22135965381363,-1.19019967921242,
-1.17501181051023,-1.16180282365541,-1.11361404212322,-1.08537774561768,
-1.065681746774,-1.01734234602368,-1.01298361676717,-0.989800484743978,
-0.975660060478834,-0.961400646454977,-0.91297299496954,-0.877560687902226,
-0.863256112850122,-0.813467002274696,-0.778613792962482,-0.758765854754386,
-0.748771882229555,-0.699694013065078,-0.665063849425104,-0.652432853856956,
-0.601574466772476,-0.567408266864309,-0.554246040117398,-0.503179057699677,
-0.47453584766665,-0.452597563304486,-0.438843075191766,-0.388240164207818,
-0.339992631709086,-0.324961067406404,-0.272319516847208,-0.244626537225397,
-0.228899959068603,-0.219677966288012),.UNSPECIFIED.);
#347=B_SPLINE_CURVE_WITH_KNOTS('',3,(#15912,#15913,#15914,#15915,#15916,
#15917,#15918,#15919,#15920,#15921,#15922,#15923,#15924,#15925,#15926,#15927,
#15928,#15929,#15930,#15931,#15932,#15933,#15934,#15935,#15936,#15937,#15938,
#15939,#15940,#15941,#15942,#15943,#15944,#15945,#15946,#15947,#15948,#15949,
#15950,#15951),.UNSPECIFIED.,.F.,.F.,(4,3,3,3,3,3,3,3,3,3,3,3,3,4),(-0.410648750432942,
-0.358826089191368,-0.328029287072579,-0.308519004108926,-0.296262202932191,
-0.26150895880243,-0.216116614902301,-0.200333794334701,-0.187454170065865,
-0.140590627549399,-0.100700164313061,-0.0879171980596439,-0.0431115726344213,
0.),.UNSPECIFIED.);
#348=B_SPLINE_CURVE_WITH_KNOTS('',3,(#15954,#15955,#15956,#15957,#15958,
#15959,#15960,#15961,#15962,#15963,#15964,#15965,#15966,#15967,#15968,#15969,
#15970,#15971,#15972),.UNSPECIFIED.,.F.,.F.,(4,3,3,3,3,3,4),(-0.219677966288012,
-0.190520484895311,-0.142890363671484,-0.122211652786797,-0.104525518218166,
-0.051044179373176,0.),.UNSPECIFIED.);
#349=B_SPLINE_CURVE_WITH_KNOTS('',3,(#16181,#16182,#16183,#16184,#16185,
#16186,#16187,#16188),.UNSPECIFIED.,.F.,.F.,(4,1,1,1,1,4),(11.6150328478183,
12.6135684378078,13.6121040277972,14.6106396177866,15.609175207776,15.707963267949),
 .UNSPECIFIED.);
#350=B_SPLINE_CURVE_WITH_KNOTS('',3,(#16189,#16190,#16191,#16192,#16193,
#16194,#16195,#16196,#16197,#16198,#16199,#16200,#16201,#16202,#16203,#16204,
#16205,#16206,#16207,#16208,#16209,#16210,#16211,#16212,#16213,#16214,#16215,
#16216,#16217,#16218,#16219,#16220,#16221,#16222,#16223,#16224,#16225,#16226,
#16227,#16228,#16229,#16230,#16231,#16232,#16233,#16234,#16235,#16236,#16237,
#16238,#16239,#16240,#16241,#16242,#16243,#16244,#16245,#16246),
 .UNSPECIFIED.,.F.,.F.,(4,3,3,3,3,3,3,3,3,3,3,3,3,3,3,3,3,3,3,4),(-0.552745378375022,
-0.531732216109367,-0.495433585222867,-0.478320891961644,-0.462732594796475,
-0.411092485600477,-0.390677853577304,-0.340757312661949,-0.30860231212099,
-0.294836984398962,-0.28154793240529,-0.252586719916514,-0.203516171016912,
-0.190166931037024,-0.142625198277768,-0.106027264752,-0.0927756455088851,
-0.0463878227544426,-0.0029163339731809,0.),.UNSPECIFIED.);
#351=B_SPLINE_CURVE_WITH_KNOTS('',3,(#16247,#16248,#16249,#16250,#16251,
#16252,#16253,#16254,#16255,#16256,#16257,#16258,#16259,#16260,#16261,#16262,
#16263,#16264,#16265),.UNSPECIFIED.,.F.,.F.,(4,3,3,3,3,3,4),(-46.4153600729827,
-45.9326371395139,-44.9341015495244,-43.935565959535,-42.9370303695455,
-41.9384947795561,-41.7920422632081),.UNSPECIFIED.);
#352=B_SPLINE_CURVE_WITH_KNOTS('',3,(#16268,#16269,#16270,#16271,#16272,
#16273,#16274,#16275,#16276),.UNSPECIFIED.,.F.,.F.,(4,1,1,1,1,1,4),(10.3761157273101,
11.3073783420651,12.3073452719531,13.3073122018412,14.3072791317292,15.3072460616173,
15.707963267949),.UNSPECIFIED.);
#353=B_SPLINE_CURVE_WITH_KNOTS('',3,(#16490,#16491,#16492,#16493,#16494,
#16495,#16496,#16497,#16498,#16499,#16500,#16501,#16502,#16503,#16504,#16505,
#16506,#16507,#16508,#16509,#16510,#16511),.UNSPECIFIED.,.F.,.F.,(4,3,3,
3,3,3,3,4),(38.8164122514459,38.9987102656334,39.9986771955214,40.9986441254095,
41.9986110552975,42.9985779851855,43.9985449150736,44.3467218980736),
 .UNSPECIFIED.);
#354=B_SPLINE_CURVE_WITH_KNOTS('',3,(#16512,#16513,#16514,#16515,#16516,
#16517,#16518,#16519,#16520,#16521,#16522,#16523,#16524,#16525,#16526,#16527,
#16528,#16529,#16530,#16531,#16532,#16533,#16534,#16535,#16536,#16537,#16538,
#16539,#16540,#16541,#16542,#16543,#16544,#16545,#16546,#16547,#16548,#16549,
#16550,#16551,#16552,#16553,#16554,#16555,#16556,#16557,#16558,#16559,#16560,
#16561,#16562,#16563,#16564,#16565,#16566),.UNSPECIFIED.,.F.,.F.,(4,3,3,
3,3,3,3,3,3,3,3,3,3,3,3,3,3,3,4),(-0.555272788399379,-0.538723215789889,
-0.502505759606931,-0.480336511409691,-0.450262499357502,-0.432260064517123,
-0.415086800376396,-0.367002820174333,-0.33403854157658,-0.315897619343378,
-0.282970454249822,-0.247599147468594,-0.225194500794938,-0.211702649714103,
-0.16177555555491,-0.11641698228548,-0.102903245473459,-0.0505012129231342,
0.),.UNSPECIFIED.);
#355=SHAPE_REPRESENTATION_RELATIONSHIP('SRR','None',#16764,#374);
#356=SHAPE_REPRESENTATION_RELATIONSHIP('SRR','None',#16765,#375);
#357=SHAPE_REPRESENTATION_RELATIONSHIP('SRR','None',#16766,#376);
#358=SHAPE_REPRESENTATION_RELATIONSHIP('SRR','None',#16767,#377);
#359=SHAPE_REPRESENTATION_RELATIONSHIP('SRR','None',#16768,#378);
#360=SHAPE_REPRESENTATION_RELATIONSHIP('SRR','None',#16769,#379);
#361=SHAPE_REPRESENTATION_RELATIONSHIP('SRR','None',#16770,#380);
#362=SHAPE_REPRESENTATION_RELATIONSHIP('SRR','None',#16771,#381);
#363=SHAPE_REPRESENTATION_RELATIONSHIP('SRR','None',#16772,#382);
#364=SHAPE_REPRESENTATION_RELATIONSHIP('SRR','None',#16773,#383);
#365=SHAPE_REPRESENTATION_RELATIONSHIP('SRR','None',#16774,#384);
#366=SHAPE_REPRESENTATION_RELATIONSHIP('SRR','None',#16775,#385);
#367=SHAPE_REPRESENTATION_RELATIONSHIP('SRR','None',#16776,#386);
#368=SHAPE_REPRESENTATION_RELATIONSHIP('SRR','None',#16777,#387);
#369=SHAPE_REPRESENTATION_RELATIONSHIP('SRR','None',#16778,#388);
#370=SHAPE_REPRESENTATION_RELATIONSHIP('SRR','None',#16779,#389);
#371=SHAPE_REPRESENTATION_RELATIONSHIP('SRR','None',#16780,#390);
#372=SHAPE_REPRESENTATION_RELATIONSHIP('SRR','None',#16781,#391);
#373=SHAPE_REPRESENTATION_RELATIONSHIP('SRR','None',#16782,#392);
#374=ADVANCED_BREP_SHAPE_REPRESENTATION('',(#412),#16668);
#375=ADVANCED_BREP_SHAPE_REPRESENTATION('',(#413),#16669);
#376=ADVANCED_BREP_SHAPE_REPRESENTATION('',(#414),#16670);
#377=ADVANCED_BREP_SHAPE_REPRESENTATION('',(#415),#16671);
#378=ADVANCED_BREP_SHAPE_REPRESENTATION('',(#416),#16672);
#379=ADVANCED_BREP_SHAPE_REPRESENTATION('',(#417),#16673);
#380=ADVANCED_BREP_SHAPE_REPRESENTATION('',(#418),#16674);
#381=ADVANCED_BREP_SHAPE_REPRESENTATION('',(#419),#16675);
#382=ADVANCED_BREP_SHAPE_REPRESENTATION('',(#420),#16676);
#383=ADVANCED_BREP_SHAPE_REPRESENTATION('',(#421),#16677);
#384=ADVANCED_BREP_SHAPE_REPRESENTATION('',(#422),#16678);
#385=ADVANCED_BREP_SHAPE_REPRESENTATION('',(#423),#16679);
#386=ADVANCED_BREP_SHAPE_REPRESENTATION('',(#424),#16680);
#387=ADVANCED_BREP_SHAPE_REPRESENTATION('',(#425),#16681);
#388=ADVANCED_BREP_SHAPE_REPRESENTATION('',(#426),#16682);
#389=ADVANCED_BREP_SHAPE_REPRESENTATION('',(#427),#16683);
#390=ADVANCED_BREP_SHAPE_REPRESENTATION('',(#428),#16684);
#391=ADVANCED_BREP_SHAPE_REPRESENTATION('',(#429),#16685);
#392=ADVANCED_BREP_SHAPE_REPRESENTATION('',(#430),#16686);
#393=STYLED_ITEM('',(#16868),#412);
#394=STYLED_ITEM('',(#16869),#413);
#395=STYLED_ITEM('',(#16870),#414);
#396=STYLED_ITEM('',(#16871),#415);
#397=STYLED_ITEM('',(#16869),#416);
#398=STYLED_ITEM('',(#16872),#417);
#399=STYLED_ITEM('',(#16868),#418);
#400=STYLED_ITEM('',(#16873),#419);
#401=STYLED_ITEM('',(#16874),#420);
#402=STYLED_ITEM('',(#16874),#421);
#403=STYLED_ITEM('',(#16874),#422);
#404=STYLED_ITEM('',(#16875),#423);
#405=STYLED_ITEM('',(#16876),#424);
#406=STYLED_ITEM('',(#16875),#425);
#407=STYLED_ITEM('',(#16877),#426);
#408=STYLED_ITEM('',(#16878),#427);
#409=STYLED_ITEM('',(#16879),#428);
#410=STYLED_ITEM('',(#16880),#429);
#411=STYLED_ITEM('',(#16881),#430);
#412=MANIFOLD_SOLID_BREP('Body1',#6112);
#413=MANIFOLD_SOLID_BREP('Body1',#6113);
#414=MANIFOLD_SOLID_BREP('Body1',#6114);
#415=MANIFOLD_SOLID_BREP('Body1',#6115);
#416=MANIFOLD_SOLID_BREP('Body1',#6116);
#417=MANIFOLD_SOLID_BREP('Body1',#6117);
#418=MANIFOLD_SOLID_BREP('Body1',#6118);
#419=MANIFOLD_SOLID_BREP('Body1',#6119);
#420=MANIFOLD_SOLID_BREP('Body1',#6120);
#421=MANIFOLD_SOLID_BREP('Body1',#6121);
#422=MANIFOLD_SOLID_BREP('Body1',#6122);
#423=MANIFOLD_SOLID_BREP('Body1',#6123);
#424=MANIFOLD_SOLID_BREP('Body1',#6124);
#425=MANIFOLD_SOLID_BREP('Body1',#6125);
#426=MANIFOLD_SOLID_BREP('Body1',#6126);
#427=MANIFOLD_SOLID_BREP('Body1',#6127);
#428=MANIFOLD_SOLID_BREP('Body1',#6128);
#429=MANIFOLD_SOLID_BREP('Body1',#6129);
#430=MANIFOLD_SOLID_BREP('Body1',#6130);
#431=FACE_BOUND('',#1036,.T.);
#432=FACE_BOUND('',#1038,.T.);
#433=FACE_BOUND('',#1078,.T.);
#434=FACE_BOUND('',#1084,.T.);
#435=FACE_BOUND('',#1085,.T.);
#436=FACE_BOUND('',#1086,.T.);
#437=FACE_BOUND('',#1087,.T.);
#438=FACE_BOUND('',#1088,.T.);
#439=FACE_BOUND('',#1089,.T.);
#440=FACE_BOUND('',#1090,.T.);
#441=FACE_BOUND('',#1094,.T.);
#442=FACE_BOUND('',#1095,.T.);
#443=FACE_BOUND('',#1096,.T.);
#444=FACE_BOUND('',#1099,.T.);
#445=FACE_BOUND('',#1100,.T.);
#446=FACE_BOUND('',#1101,.T.);
#447=FACE_BOUND('',#1102,.T.);
#448=FACE_BOUND('',#1103,.T.);
#449=FACE_BOUND('',#1105,.T.);
#450=FACE_BOUND('',#1106,.T.);
#451=FACE_BOUND('',#1107,.T.);
#452=FACE_BOUND('',#1108,.T.);
#453=FACE_BOUND('',#1109,.T.);
#454=FACE_BOUND('',#1113,.T.);
#455=FACE_BOUND('',#1115,.T.);
#456=FACE_BOUND('',#1123,.T.);
#457=FACE_BOUND('',#1124,.T.);
#458=FACE_BOUND('',#1125,.T.);
#459=FACE_BOUND('',#1126,.T.);
#460=FACE_BOUND('',#1127,.T.);
#461=FACE_BOUND('',#1129,.T.);
#462=FACE_BOUND('',#1130,.T.);
#463=FACE_BOUND('',#1131,.T.);
#464=FACE_BOUND('',#1132,.T.);
#465=FACE_BOUND('',#1133,.T.);
#466=FACE_BOUND('',#1139,.T.);
#467=FACE_BOUND('',#1140,.T.);
#468=FACE_BOUND('',#1141,.T.);
#469=FACE_BOUND('',#1142,.T.);
#470=FACE_BOUND('',#1143,.T.);
#471=FACE_BOUND('',#1144,.T.);
#472=FACE_BOUND('',#1145,.T.);
#473=FACE_BOUND('',#1178,.T.);
#474=FACE_BOUND('',#1182,.T.);
#475=FACE_BOUND('',#1186,.T.);
#476=FACE_BOUND('',#1188,.T.);
#477=FACE_BOUND('',#1256,.T.);
#478=FACE_BOUND('',#1258,.T.);
#479=FACE_BOUND('',#1259,.T.);
#480=FACE_BOUND('',#1260,.T.);
#481=FACE_BOUND('',#1261,.T.);
#482=FACE_BOUND('',#1266,.T.);
#483=FACE_BOUND('',#1267,.T.);
#484=FACE_BOUND('',#1268,.T.);
#485=FACE_BOUND('',#1269,.T.);
#486=FACE_BOUND('',#1270,.T.);
#487=FACE_BOUND('',#1289,.T.);
#488=FACE_BOUND('',#1290,.T.);
#489=FACE_BOUND('',#1291,.T.);
#490=FACE_BOUND('',#1292,.T.);
#491=FACE_BOUND('',#1293,.T.);
#492=FACE_BOUND('',#1296,.T.);
#493=FACE_BOUND('',#1297,.T.);
#494=FACE_BOUND('',#1298,.T.);
#495=FACE_BOUND('',#1299,.T.);
#496=FACE_BOUND('',#1300,.T.);
#497=FACE_BOUND('',#1308,.T.);
#498=FACE_BOUND('',#1315,.T.);
#499=FACE_BOUND('',#1316,.T.);
#500=FACE_BOUND('',#1317,.T.);
#501=FACE_BOUND('',#1318,.T.);
#502=FACE_BOUND('',#1319,.T.);
#503=FACE_BOUND('',#1324,.T.);
#504=FACE_BOUND('',#1325,.T.);
#505=FACE_BOUND('',#1326,.T.);
#506=FACE_BOUND('',#1327,.T.);
#507=FACE_BOUND('',#1328,.T.);
#508=FACE_BOUND('',#1334,.T.);
#509=FACE_BOUND('',#1335,.T.);
#510=FACE_BOUND('',#1336,.T.);
#511=FACE_BOUND('',#1337,.T.);
#512=FACE_BOUND('',#1338,.T.);
#513=FACE_BOUND('',#1341,.T.);
#514=FACE_BOUND('',#1347,.T.);
#515=FACE_BOUND('',#1354,.T.);
#516=FACE_BOUND('',#1356,.T.);
#517=FACE_BOUND('',#1360,.T.);
#518=FACE_BOUND('',#1362,.T.);
#519=FACE_BOUND('',#1365,.T.);
#520=FACE_BOUND('',#1366,.T.);
#521=FACE_BOUND('',#1367,.T.);
#522=FACE_BOUND('',#1368,.T.);
#523=FACE_BOUND('',#1369,.T.);
#524=FACE_BOUND('',#1371,.T.);
#525=FACE_BOUND('',#1372,.T.);
#526=FACE_BOUND('',#1373,.T.);
#527=FACE_BOUND('',#1374,.T.);
#528=FACE_BOUND('',#1375,.T.);
#529=FACE_BOUND('',#1395,.T.);
#530=FACE_BOUND('',#1397,.T.);
#531=FACE_BOUND('',#1399,.T.);
#532=FACE_BOUND('',#1401,.T.);
#533=FACE_BOUND('',#1405,.T.);
#534=FACE_BOUND('',#1406,.T.);
#535=FACE_BOUND('',#1412,.T.);
#536=FACE_BOUND('',#1414,.T.);
#537=FACE_BOUND('',#1418,.T.);
#538=FACE_BOUND('',#1420,.T.);
#539=FACE_BOUND('',#1424,.T.);
#540=FACE_BOUND('',#1426,.T.);
#541=FACE_BOUND('',#1430,.T.);
#542=FACE_BOUND('',#1432,.T.);
#543=FACE_BOUND('',#1442,.T.);
#544=FACE_BOUND('',#1444,.T.);
#545=FACE_BOUND('',#1448,.T.);
#546=FACE_BOUND('',#1450,.T.);
#547=FACE_BOUND('',#1454,.T.);
#548=FACE_BOUND('',#1456,.T.);
#549=FACE_BOUND('',#1460,.T.);
#550=FACE_BOUND('',#1462,.T.);
#551=FACE_BOUND('',#1497,.T.);
#552=FACE_BOUND('',#1500,.T.);
#553=PLANE('',#6349);
#554=PLANE('',#6350);
#555=PLANE('',#6364);
#556=PLANE('',#6368);
#557=PLANE('',#6372);
#558=PLANE('',#6373);
#559=PLANE('',#6377);
#560=PLANE('',#6381);
#561=PLANE('',#6382);
#562=PLANE('',#6386);
#563=PLANE('',#6390);
#564=PLANE('',#6391);
#565=PLANE('',#6395);
#566=PLANE('',#6399);
#567=PLANE('',#6400);
#568=PLANE('',#6404);
#569=PLANE('',#6408);
#570=PLANE('',#6409);
#571=PLANE('',#6413);
#572=PLANE('',#6417);
#573=PLANE('',#6418);
#574=PLANE('',#6419);
#575=PLANE('',#6420);
#576=PLANE('',#6421);
#577=PLANE('',#6422);
#578=PLANE('',#6438);
#579=PLANE('',#6442);
#580=PLANE('',#6443);
#581=PLANE('',#6449);
#582=PLANE('',#6450);
#583=PLANE('',#6458);
#584=PLANE('',#6459);
#585=PLANE('',#6478);
#586=PLANE('',#6479);
#587=PLANE('',#6481);
#588=PLANE('',#6482);
#589=PLANE('',#6483);
#590=PLANE('',#6484);
#591=PLANE('',#6486);
#592=PLANE('',#6504);
#593=PLANE('',#6507);
#594=PLANE('',#6508);
#595=PLANE('',#6511);
#596=PLANE('',#6514);
#597=PLANE('',#6515);
#598=PLANE('',#6518);
#599=PLANE('',#6521);
#600=PLANE('',#6522);
#601=PLANE('',#6525);
#602=PLANE('',#6528);
#603=PLANE('',#6529);
#604=PLANE('',#6532);
#605=PLANE('',#6535);
#606=PLANE('',#6536);
#607=PLANE('',#6539);
#608=PLANE('',#6542);
#609=PLANE('',#6543);
#610=PLANE('',#6547);
#611=PLANE('',#6552);
#612=PLANE('',#6560);
#613=PLANE('',#6561);
#614=PLANE('',#6649);
#615=PLANE('',#6650);
#616=PLANE('',#6660);
#617=PLANE('',#6682);
#618=PLANE('',#6687);
#619=PLANE('',#6690);
#620=PLANE('',#6691);
#621=PLANE('',#6692);
#622=PLANE('',#6693);
#623=PLANE('',#6698);
#624=PLANE('',#6707);
#625=PLANE('',#6708);
#626=PLANE('',#6710);
#627=PLANE('',#6716);
#628=PLANE('',#6731);
#629=PLANE('',#6735);
#630=PLANE('',#6763);
#631=PLANE('',#6765);
#632=PLANE('',#6772);
#633=PLANE('',#6773);
#634=PLANE('',#6776);
#635=PLANE('',#6777);
#636=PLANE('',#6783);
#637=PLANE('',#6786);
#638=PLANE('',#6787);
#639=PLANE('',#6792);
#640=PLANE('',#6795);
#641=PLANE('',#6798);
#642=PLANE('',#6799);
#643=PLANE('',#6802);
#644=PLANE('',#6805);
#645=PLANE('',#6809);
#646=PLANE('',#6811);
#647=PLANE('',#6812);
#648=PLANE('',#6815);
#649=PLANE('',#6822);
#650=PLANE('',#6823);
#651=PLANE('',#6831);
#652=PLANE('',#6832);
#653=PLANE('',#6840);
#654=PLANE('',#6841);
#655=PLANE('',#6849);
#656=PLANE('',#6850);
#657=PLANE('',#6858);
#658=PLANE('',#6859);
#659=PLANE('',#6861);
#660=PLANE('',#6865);
#661=PLANE('',#6869);
#662=PLANE('',#6870);
#663=PLANE('',#6878);
#664=PLANE('',#6879);
#665=PLANE('',#6887);
#666=PLANE('',#6888);
#667=PLANE('',#6896);
#668=PLANE('',#6897);
#669=PLANE('',#6905);
#670=PLANE('',#6906);
#671=PLANE('',#6908);
#672=PLANE('',#6909);
#673=PLANE('',#6910);
#674=PLANE('',#6917);
#675=PLANE('',#6942);
#676=PLANE('',#6944);
#677=PLANE('',#6945);
#678=PLANE('',#6946);
#679=PLANE('',#6947);
#680=PLANE('',#6948);
#681=PLANE('',#6949);
#682=PLANE('',#6950);
#683=PLANE('',#6951);
#684=PLANE('',#6955);
#685=PLANE('',#6956);
#686=FACE_OUTER_BOUND('',#1033,.T.);
#687=FACE_OUTER_BOUND('',#1034,.T.);
#688=FACE_OUTER_BOUND('',#1035,.T.);
#689=FACE_OUTER_BOUND('',#1037,.T.);
#690=FACE_OUTER_BOUND('',#1039,.T.);
#691=FACE_OUTER_BOUND('',#1040,.T.);
#692=FACE_OUTER_BOUND('',#1041,.T.);
#693=FACE_OUTER_BOUND('',#1042,.T.);
#694=FACE_OUTER_BOUND('',#1043,.T.);
#695=FACE_OUTER_BOUND('',#1044,.T.);
#696=FACE_OUTER_BOUND('',#1045,.T.);
#697=FACE_OUTER_BOUND('',#1046,.T.);
#698=FACE_OUTER_BOUND('',#1047,.T.);
#699=FACE_OUTER_BOUND('',#1048,.T.);
#700=FACE_OUTER_BOUND('',#1049,.T.);
#701=FACE_OUTER_BOUND('',#1050,.T.);
#702=FACE_OUTER_BOUND('',#1051,.T.);
#703=FACE_OUTER_BOUND('',#1052,.T.);
#704=FACE_OUTER_BOUND('',#1053,.T.);
#705=FACE_OUTER_BOUND('',#1054,.T.);
#706=FACE_OUTER_BOUND('',#1055,.T.);
#707=FACE_OUTER_BOUND('',#1056,.T.);
#708=FACE_OUTER_BOUND('',#1057,.T.);
#709=FACE_OUTER_BOUND('',#1058,.T.);
#710=FACE_OUTER_BOUND('',#1059,.T.);
#711=FACE_OUTER_BOUND('',#1060,.T.);
#712=FACE_OUTER_BOUND('',#1061,.T.);
#713=FACE_OUTER_BOUND('',#1062,.T.);
#714=FACE_OUTER_BOUND('',#1063,.T.);
#715=FACE_OUTER_BOUND('',#1064,.T.);
#716=FACE_OUTER_BOUND('',#1065,.T.);
#717=FACE_OUTER_BOUND('',#1066,.T.);
#718=FACE_OUTER_BOUND('',#1067,.T.);
#719=FACE_OUTER_BOUND('',#1068,.T.);
#720=FACE_OUTER_BOUND('',#1069,.T.);
#721=FACE_OUTER_BOUND('',#1070,.T.);
#722=FACE_OUTER_BOUND('',#1071,.T.);
#723=FACE_OUTER_BOUND('',#1072,.T.);
#724=FACE_OUTER_BOUND('',#1073,.T.);
#725=FACE_OUTER_BOUND('',#1074,.T.);
#726=FACE_OUTER_BOUND('',#1075,.T.);
#727=FACE_OUTER_BOUND('',#1076,.T.);
#728=FACE_OUTER_BOUND('',#1077,.T.);
#729=FACE_OUTER_BOUND('',#1079,.T.);
#730=FACE_OUTER_BOUND('',#1080,.T.);
#731=FACE_OUTER_BOUND('',#1081,.T.);
#732=FACE_OUTER_BOUND('',#1082,.T.);
#733=FACE_OUTER_BOUND('',#1083,.T.);
#734=FACE_OUTER_BOUND('',#1091,.T.);
#735=FACE_OUTER_BOUND('',#1092,.T.);
#736=FACE_OUTER_BOUND('',#1093,.T.);
#737=FACE_OUTER_BOUND('',#1097,.T.);
#738=FACE_OUTER_BOUND('',#1098,.T.);
#739=FACE_OUTER_BOUND('',#1104,.T.);
#740=FACE_OUTER_BOUND('',#1110,.T.);
#741=FACE_OUTER_BOUND('',#1111,.T.);
#742=FACE_OUTER_BOUND('',#1112,.T.);
#743=FACE_OUTER_BOUND('',#1114,.T.);
#744=FACE_OUTER_BOUND('',#1116,.T.);
#745=FACE_OUTER_BOUND('',#1117,.T.);
#746=FACE_OUTER_BOUND('',#1118,.T.);
#747=FACE_OUTER_BOUND('',#1119,.T.);
#748=FACE_OUTER_BOUND('',#1120,.T.);
#749=FACE_OUTER_BOUND('',#1121,.T.);
#750=FACE_OUTER_BOUND('',#1122,.T.);
#751=FACE_OUTER_BOUND('',#1128,.T.);
#752=FACE_OUTER_BOUND('',#1134,.T.);
#753=FACE_OUTER_BOUND('',#1135,.T.);
#754=FACE_OUTER_BOUND('',#1136,.T.);
#755=FACE_OUTER_BOUND('',#1137,.T.);
#756=FACE_OUTER_BOUND('',#1138,.T.);
#757=FACE_OUTER_BOUND('',#1146,.T.);
#758=FACE_OUTER_BOUND('',#1147,.T.);
#759=FACE_OUTER_BOUND('',#1148,.T.);
#760=FACE_OUTER_BOUND('',#1149,.T.);
#761=FACE_OUTER_BOUND('',#1150,.T.);
#762=FACE_OUTER_BOUND('',#1151,.T.);
#763=FACE_OUTER_BOUND('',#1152,.T.);
#764=FACE_OUTER_BOUND('',#1153,.T.);
#765=FACE_OUTER_BOUND('',#1154,.T.);
#766=FACE_OUTER_BOUND('',#1155,.T.);
#767=FACE_OUTER_BOUND('',#1156,.T.);
#768=FACE_OUTER_BOUND('',#1157,.T.);
#769=FACE_OUTER_BOUND('',#1158,.T.);
#770=FACE_OUTER_BOUND('',#1159,.T.);
#771=FACE_OUTER_BOUND('',#1160,.T.);
#772=FACE_OUTER_BOUND('',#1161,.T.);
#773=FACE_OUTER_BOUND('',#1162,.T.);
#774=FACE_OUTER_BOUND('',#1163,.T.);
#775=FACE_OUTER_BOUND('',#1164,.T.);
#776=FACE_OUTER_BOUND('',#1165,.T.);
#777=FACE_OUTER_BOUND('',#1166,.T.);
#778=FACE_OUTER_BOUND('',#1167,.T.);
#779=FACE_OUTER_BOUND('',#1168,.T.);
#780=FACE_OUTER_BOUND('',#1169,.T.);
#781=FACE_OUTER_BOUND('',#1170,.T.);
#782=FACE_OUTER_BOUND('',#1171,.T.);
#783=FACE_OUTER_BOUND('',#1172,.T.);
#784=FACE_OUTER_BOUND('',#1173,.T.);
#785=FACE_OUTER_BOUND('',#1174,.T.);
#786=FACE_OUTER_BOUND('',#1175,.T.);
#787=FACE_OUTER_BOUND('',#1176,.T.);
#788=FACE_OUTER_BOUND('',#1177,.T.);
#789=FACE_OUTER_BOUND('',#1179,.T.);
#790=FACE_OUTER_BOUND('',#1180,.T.);
#791=FACE_OUTER_BOUND('',#1181,.T.);
#792=FACE_OUTER_BOUND('',#1183,.T.);
#793=FACE_OUTER_BOUND('',#1184,.T.);
#794=FACE_OUTER_BOUND('',#1185,.T.);
#795=FACE_OUTER_BOUND('',#1187,.T.);
#796=FACE_OUTER_BOUND('',#1189,.T.);
#797=FACE_OUTER_BOUND('',#1190,.T.);
#798=FACE_OUTER_BOUND('',#1191,.T.);
#799=FACE_OUTER_BOUND('',#1192,.T.);
#800=FACE_OUTER_BOUND('',#1193,.T.);
#801=FACE_OUTER_BOUND('',#1194,.T.);
#802=FACE_OUTER_BOUND('',#1195,.T.);
#803=FACE_OUTER_BOUND('',#1196,.T.);
#804=FACE_OUTER_BOUND('',#1197,.T.);
#805=FACE_OUTER_BOUND('',#1198,.T.);
#806=FACE_OUTER_BOUND('',#1199,.T.);
#807=FACE_OUTER_BOUND('',#1200,.T.);
#808=FACE_OUTER_BOUND('',#1201,.T.);
#809=FACE_OUTER_BOUND('',#1202,.T.);
#810=FACE_OUTER_BOUND('',#1203,.T.);
#811=FACE_OUTER_BOUND('',#1204,.T.);
#812=FACE_OUTER_BOUND('',#1205,.T.);
#813=FACE_OUTER_BOUND('',#1206,.T.);
#814=FACE_OUTER_BOUND('',#1207,.T.);
#815=FACE_OUTER_BOUND('',#1208,.T.);
#816=FACE_OUTER_BOUND('',#1209,.T.);
#817=FACE_OUTER_BOUND('',#1210,.T.);
#818=FACE_OUTER_BOUND('',#1211,.T.);
#819=FACE_OUTER_BOUND('',#1212,.T.);
#820=FACE_OUTER_BOUND('',#1213,.T.);
#821=FACE_OUTER_BOUND('',#1214,.T.);
#822=FACE_OUTER_BOUND('',#1215,.T.);
#823=FACE_OUTER_BOUND('',#1216,.T.);
#824=FACE_OUTER_BOUND('',#1217,.T.);
#825=FACE_OUTER_BOUND('',#1218,.T.);
#826=FACE_OUTER_BOUND('',#1219,.T.);
#827=FACE_OUTER_BOUND('',#1220,.T.);
#828=FACE_OUTER_BOUND('',#1221,.T.);
#829=FACE_OUTER_BOUND('',#1222,.T.);
#830=FACE_OUTER_BOUND('',#1223,.T.);
#831=FACE_OUTER_BOUND('',#1224,.T.);
#832=FACE_OUTER_BOUND('',#1225,.T.);
#833=FACE_OUTER_BOUND('',#1226,.T.);
#834=FACE_OUTER_BOUND('',#1227,.T.);
#835=FACE_OUTER_BOUND('',#1228,.T.);
#836=FACE_OUTER_BOUND('',#1229,.T.);
#837=FACE_OUTER_BOUND('',#1230,.T.);
#838=FACE_OUTER_BOUND('',#1231,.T.);
#839=FACE_OUTER_BOUND('',#1232,.T.);
#840=FACE_OUTER_BOUND('',#1233,.T.);
#841=FACE_OUTER_BOUND('',#1234,.T.);
#842=FACE_OUTER_BOUND('',#1235,.T.);
#843=FACE_OUTER_BOUND('',#1236,.T.);
#844=FACE_OUTER_BOUND('',#1237,.T.);
#845=FACE_OUTER_BOUND('',#1238,.T.);
#846=FACE_OUTER_BOUND('',#1239,.T.);
#847=FACE_OUTER_BOUND('',#1240,.T.);
#848=FACE_OUTER_BOUND('',#1241,.T.);
#849=FACE_OUTER_BOUND('',#1242,.T.);
#850=FACE_OUTER_BOUND('',#1243,.T.);
#851=FACE_OUTER_BOUND('',#1244,.T.);
#852=FACE_OUTER_BOUND('',#1245,.T.);
#853=FACE_OUTER_BOUND('',#1246,.T.);
#854=FACE_OUTER_BOUND('',#1247,.T.);
#855=FACE_OUTER_BOUND('',#1248,.T.);
#856=FACE_OUTER_BOUND('',#1249,.T.);
#857=FACE_OUTER_BOUND('',#1250,.T.);
#858=FACE_OUTER_BOUND('',#1251,.T.);
#859=FACE_OUTER_BOUND('',#1252,.T.);
#860=FACE_OUTER_BOUND('',#1253,.T.);
#861=FACE_OUTER_BOUND('',#1254,.T.);
#862=FACE_OUTER_BOUND('',#1255,.T.);
#863=FACE_OUTER_BOUND('',#1257,.T.);
#864=FACE_OUTER_BOUND('',#1262,.T.);
#865=FACE_OUTER_BOUND('',#1263,.T.);
#866=FACE_OUTER_BOUND('',#1264,.T.);
#867=FACE_OUTER_BOUND('',#1265,.T.);
#868=FACE_OUTER_BOUND('',#1271,.T.);
#869=FACE_OUTER_BOUND('',#1272,.T.);
#870=FACE_OUTER_BOUND('',#1273,.T.);
#871=FACE_OUTER_BOUND('',#1274,.T.);
#872=FACE_OUTER_BOUND('',#1275,.T.);
#873=FACE_OUTER_BOUND('',#1276,.T.);
#874=FACE_OUTER_BOUND('',#1277,.T.);
#875=FACE_OUTER_BOUND('',#1278,.T.);
#876=FACE_OUTER_BOUND('',#1279,.T.);
#877=FACE_OUTER_BOUND('',#1280,.T.);
#878=FACE_OUTER_BOUND('',#1281,.T.);
#879=FACE_OUTER_BOUND('',#1282,.T.);
#880=FACE_OUTER_BOUND('',#1283,.T.);
#881=FACE_OUTER_BOUND('',#1284,.T.);
#882=FACE_OUTER_BOUND('',#1285,.T.);
#883=FACE_OUTER_BOUND('',#1286,.T.);
#884=FACE_OUTER_BOUND('',#1287,.T.);
#885=FACE_OUTER_BOUND('',#1288,.T.);
#886=FACE_OUTER_BOUND('',#1294,.T.);
#887=FACE_OUTER_BOUND('',#1295,.T.);
#888=FACE_OUTER_BOUND('',#1301,.T.);
#889=FACE_OUTER_BOUND('',#1302,.T.);
#890=FACE_OUTER_BOUND('',#1303,.T.);
#891=FACE_OUTER_BOUND('',#1304,.T.);
#892=FACE_OUTER_BOUND('',#1305,.T.);
#893=FACE_OUTER_BOUND('',#1306,.T.);
#894=FACE_OUTER_BOUND('',#1307,.T.);
#895=FACE_OUTER_BOUND('',#1309,.T.);
#896=FACE_OUTER_BOUND('',#1310,.T.);
#897=FACE_OUTER_BOUND('',#1311,.T.);
#898=FACE_OUTER_BOUND('',#1312,.T.);
#899=FACE_OUTER_BOUND('',#1313,.T.);
#900=FACE_OUTER_BOUND('',#1314,.T.);
#901=FACE_OUTER_BOUND('',#1320,.T.);
#902=FACE_OUTER_BOUND('',#1321,.T.);
#903=FACE_OUTER_BOUND('',#1322,.T.);
#904=FACE_OUTER_BOUND('',#1323,.T.);
#905=FACE_OUTER_BOUND('',#1329,.T.);
#906=FACE_OUTER_BOUND('',#1330,.T.);
#907=FACE_OUTER_BOUND('',#1331,.T.);
#908=FACE_OUTER_BOUND('',#1332,.T.);
#909=FACE_OUTER_BOUND('',#1333,.T.);
#910=FACE_OUTER_BOUND('',#1339,.T.);
#911=FACE_OUTER_BOUND('',#1340,.T.);
#912=FACE_OUTER_BOUND('',#1342,.T.);
#913=FACE_OUTER_BOUND('',#1343,.T.);
#914=FACE_OUTER_BOUND('',#1344,.T.);
#915=FACE_OUTER_BOUND('',#1345,.T.);
#916=FACE_OUTER_BOUND('',#1346,.T.);
#917=FACE_OUTER_BOUND('',#1348,.T.);
#918=FACE_OUTER_BOUND('',#1349,.T.);
#919=FACE_OUTER_BOUND('',#1350,.T.);
#920=FACE_OUTER_BOUND('',#1351,.T.);
#921=FACE_OUTER_BOUND('',#1352,.T.);
#922=FACE_OUTER_BOUND('',#1353,.T.);
#923=FACE_OUTER_BOUND('',#1355,.T.);
#924=FACE_OUTER_BOUND('',#1357,.T.);
#925=FACE_OUTER_BOUND('',#1358,.T.);
#926=FACE_OUTER_BOUND('',#1359,.T.);
#927=FACE_OUTER_BOUND('',#1361,.T.);
#928=FACE_OUTER_BOUND('',#1363,.T.);
#929=FACE_OUTER_BOUND('',#1364,.T.);
#930=FACE_OUTER_BOUND('',#1370,.T.);
#931=FACE_OUTER_BOUND('',#1376,.T.);
#932=FACE_OUTER_BOUND('',#1377,.T.);
#933=FACE_OUTER_BOUND('',#1378,.T.);
#934=FACE_OUTER_BOUND('',#1379,.T.);
#935=FACE_OUTER_BOUND('',#1380,.T.);
#936=FACE_OUTER_BOUND('',#1381,.T.);
#937=FACE_OUTER_BOUND('',#1382,.T.);
#938=FACE_OUTER_BOUND('',#1383,.T.);
#939=FACE_OUTER_BOUND('',#1384,.T.);
#940=FACE_OUTER_BOUND('',#1385,.T.);
#941=FACE_OUTER_BOUND('',#1386,.T.);
#942=FACE_OUTER_BOUND('',#1387,.T.);
#943=FACE_OUTER_BOUND('',#1388,.T.);
#944=FACE_OUTER_BOUND('',#1389,.T.);
#945=FACE_OUTER_BOUND('',#1390,.T.);
#946=FACE_OUTER_BOUND('',#1391,.T.);
#947=FACE_OUTER_BOUND('',#1392,.T.);
#948=FACE_OUTER_BOUND('',#1393,.T.);
#949=FACE_OUTER_BOUND('',#1394,.T.);
#950=FACE_OUTER_BOUND('',#1396,.T.);
#951=FACE_OUTER_BOUND('',#1398,.T.);
#952=FACE_OUTER_BOUND('',#1400,.T.);
#953=FACE_OUTER_BOUND('',#1402,.T.);
#954=FACE_OUTER_BOUND('',#1403,.T.);
#955=FACE_OUTER_BOUND('',#1404,.T.);
#956=FACE_OUTER_BOUND('',#1407,.T.);
#957=FACE_OUTER_BOUND('',#1408,.T.);
#958=FACE_OUTER_BOUND('',#1409,.T.);
#959=FACE_OUTER_BOUND('',#1410,.T.);
#960=FACE_OUTER_BOUND('',#1411,.T.);
#961=FACE_OUTER_BOUND('',#1413,.T.);
#962=FACE_OUTER_BOUND('',#1415,.T.);
#963=FACE_OUTER_BOUND('',#1416,.T.);
#964=FACE_OUTER_BOUND('',#1417,.T.);
#965=FACE_OUTER_BOUND('',#1419,.T.);
#966=FACE_OUTER_BOUND('',#1421,.T.);
#967=FACE_OUTER_BOUND('',#1422,.T.);
#968=FACE_OUTER_BOUND('',#1423,.T.);
#969=FACE_OUTER_BOUND('',#1425,.T.);
#970=FACE_OUTER_BOUND('',#1427,.T.);
#971=FACE_OUTER_BOUND('',#1428,.T.);
#972=FACE_OUTER_BOUND('',#1429,.T.);
#973=FACE_OUTER_BOUND('',#1431,.T.);
#974=FACE_OUTER_BOUND('',#1433,.T.);
#975=FACE_OUTER_BOUND('',#1434,.T.);
#976=FACE_OUTER_BOUND('',#1435,.T.);
#977=FACE_OUTER_BOUND('',#1436,.T.);
#978=FACE_OUTER_BOUND('',#1437,.T.);
#979=FACE_OUTER_BOUND('',#1438,.T.);
#980=FACE_OUTER_BOUND('',#1439,.T.);
#981=FACE_OUTER_BOUND('',#1440,.T.);
#982=FACE_OUTER_BOUND('',#1441,.T.);
#983=FACE_OUTER_BOUND('',#1443,.T.);
#984=FACE_OUTER_BOUND('',#1445,.T.);
#985=FACE_OUTER_BOUND('',#1446,.T.);
#986=FACE_OUTER_BOUND('',#1447,.T.);
#987=FACE_OUTER_BOUND('',#1449,.T.);
#988=FACE_OUTER_BOUND('',#1451,.T.);
#989=FACE_OUTER_BOUND('',#1452,.T.);
#990=FACE_OUTER_BOUND('',#1453,.T.);
#991=FACE_OUTER_BOUND('',#1455,.T.);
#992=FACE_OUTER_BOUND('',#1457,.T.);
#993=FACE_OUTER_BOUND('',#1458,.T.);
#994=FACE_OUTER_BOUND('',#1459,.T.);
#995=FACE_OUTER_BOUND('',#1461,.T.);
#996=FACE_OUTER_BOUND('',#1463,.T.);
#997=FACE_OUTER_BOUND('',#1464,.T.);
#998=FACE_OUTER_BOUND('',#1465,.T.);
#999=FACE_OUTER_BOUND('',#1466,.T.);
#1000=FACE_OUTER_BOUND('',#1467,.T.);
#1001=FACE_OUTER_BOUND('',#1468,.T.);
#1002=FACE_OUTER_BOUND('',#1469,.T.);
#1003=FACE_OUTER_BOUND('',#1470,.T.);
#1004=FACE_OUTER_BOUND('',#1471,.T.);
#1005=FACE_OUTER_BOUND('',#1472,.T.);
#1006=FACE_OUTER_BOUND('',#1473,.T.);
#1007=FACE_OUTER_BOUND('',#1474,.T.);
#1008=FACE_OUTER_BOUND('',#1475,.T.);
#1009=FACE_OUTER_BOUND('',#1476,.T.);
#1010=FACE_OUTER_BOUND('',#1477,.T.);
#1011=FACE_OUTER_BOUND('',#1478,.T.);
#1012=FACE_OUTER_BOUND('',#1479,.T.);
#1013=FACE_OUTER_BOUND('',#1480,.T.);
#1014=FACE_OUTER_BOUND('',#1481,.T.);
#1015=FACE_OUTER_BOUND('',#1482,.T.);
#1016=FACE_OUTER_BOUND('',#1483,.T.);
#1017=FACE_OUTER_BOUND('',#1484,.T.);
#1018=FACE_OUTER_BOUND('',#1485,.T.);
#1019=FACE_OUTER_BOUND('',#1486,.T.);
#1020=FACE_OUTER_BOUND('',#1487,.T.);
#1021=FACE_OUTER_BOUND('',#1488,.T.);
#1022=FACE_OUTER_BOUND('',#1489,.T.);
#1023=FACE_OUTER_BOUND('',#1490,.T.);
#1024=FACE_OUTER_BOUND('',#1491,.T.);
#1025=FACE_OUTER_BOUND('',#1492,.T.);
#1026=FACE_OUTER_BOUND('',#1493,.T.);
#1027=FACE_OUTER_BOUND('',#1494,.T.);
#1028=FACE_OUTER_BOUND('',#1495,.T.);
#1029=FACE_OUTER_BOUND('',#1496,.T.);
#1030=FACE_OUTER_BOUND('',#1498,.T.);
#1031=FACE_OUTER_BOUND('',#1499,.T.);
#1032=FACE_OUTER_BOUND('',#1501,.T.);
#1033=EDGE_LOOP('',(#3891,#3892,#3893,#3894));
#1034=EDGE_LOOP('',(#3895,#3896,#3897,#3898));
#1035=EDGE_LOOP('',(#3899));
#1036=EDGE_LOOP('',(#3900));
#1037=EDGE_LOOP('',(#3901));
#1038=EDGE_LOOP('',(#3902));
#1039=EDGE_LOOP('',(#3903,#3904,#3905,#3906));
#1040=EDGE_LOOP('',(#3907,#3908,#3909,#3910));
#1041=EDGE_LOOP('',(#3911,#3912,#3913,#3914));
#1042=EDGE_LOOP('',(#3915,#3916,#3917,#3918));
#1043=EDGE_LOOP('',(#3919,#3920,#3921,#3922));
#1044=EDGE_LOOP('',(#3923,#3924,#3925,#3926));
#1045=EDGE_LOOP('',(#3927,#3928,#3929,#3930));
#1046=EDGE_LOOP('',(#3931,#3932,#3933,#3934));
#1047=EDGE_LOOP('',(#3935,#3936,#3937,#3938));
#1048=EDGE_LOOP('',(#3939,#3940,#3941,#3942));
#1049=EDGE_LOOP('',(#3943,#3944,#3945,#3946));
#1050=EDGE_LOOP('',(#3947,#3948,#3949,#3950));
#1051=EDGE_LOOP('',(#3951,#3952,#3953,#3954));
#1052=EDGE_LOOP('',(#3955,#3956,#3957,#3958));
#1053=EDGE_LOOP('',(#3959,#3960,#3961,#3962));
#1054=EDGE_LOOP('',(#3963,#3964,#3965,#3966));
#1055=EDGE_LOOP('',(#3967,#3968,#3969,#3970));
#1056=EDGE_LOOP('',(#3971,#3972,#3973,#3974));
#1057=EDGE_LOOP('',(#3975,#3976,#3977,#3978));
#1058=EDGE_LOOP('',(#3979,#3980,#3981,#3982));
#1059=EDGE_LOOP('',(#3983,#3984,#3985,#3986));
#1060=EDGE_LOOP('',(#3987,#3988,#3989,#3990));
#1061=EDGE_LOOP('',(#3991,#3992,#3993,#3994));
#1062=EDGE_LOOP('',(#3995,#3996,#3997,#3998));
#1063=EDGE_LOOP('',(#3999,#4000,#4001,#4002));
#1064=EDGE_LOOP('',(#4003,#4004,#4005,#4006));
#1065=EDGE_LOOP('',(#4007,#4008,#4009,#4010));
#1066=EDGE_LOOP('',(#4011,#4012,#4013,#4014));
#1067=EDGE_LOOP('',(#4015,#4016,#4017,#4018));
#1068=EDGE_LOOP('',(#4019,#4020,#4021,#4022));
#1069=EDGE_LOOP('',(#4023,#4024,#4025,#4026));
#1070=EDGE_LOOP('',(#4027,#4028,#4029,#4030));
#1071=EDGE_LOOP('',(#4031,#4032,#4033,#4034));
#1072=EDGE_LOOP('',(#4035,#4036,#4037,#4038));
#1073=EDGE_LOOP('',(#4039,#4040,#4041,#4042));
#1074=EDGE_LOOP('',(#4043,#4044,#4045,#4046));
#1075=EDGE_LOOP('',(#4047,#4048,#4049,#4050));
#1076=EDGE_LOOP('',(#4051,#4052,#4053,#4054));
#1077=EDGE_LOOP('',(#4055,#4056,#4057,#4058,#4059,#4060,#4061,#4062,#4063,
#4064,#4065,#4066));
#1078=EDGE_LOOP('',(#4067));
#1079=EDGE_LOOP('',(#4068,#4069,#4070,#4071));
#1080=EDGE_LOOP('',(#4072,#4073,#4074,#4075));
#1081=EDGE_LOOP('',(#4076,#4077,#4078,#4079));
#1082=EDGE_LOOP('',(#4080,#4081,#4082,#4083));
#1083=EDGE_LOOP('',(#4084,#4085,#4086,#4087,#4088,#4089,#4090,#4091,#4092,
#4093,#4094,#4095));
#1084=EDGE_LOOP('',(#4096));
#1085=EDGE_LOOP('',(#4097,#4098,#4099,#4100));
#1086=EDGE_LOOP('',(#4101,#4102,#4103,#4104));
#1087=EDGE_LOOP('',(#4105,#4106,#4107,#4108));
#1088=EDGE_LOOP('',(#4109,#4110,#4111,#4112));
#1089=EDGE_LOOP('',(#4113,#4114,#4115,#4116));
#1090=EDGE_LOOP('',(#4117,#4118,#4119,#4120));
#1091=EDGE_LOOP('',(#4121,#4122,#4123,#4124));
#1092=EDGE_LOOP('',(#4125,#4126,#4127,#4128));
#1093=EDGE_LOOP('',(#4129,#4130,#4131,#4132));
#1094=EDGE_LOOP('',(#4133,#4134,#4135,#4136));
#1095=EDGE_LOOP('',(#4137,#4138,#4139,#4140));
#1096=EDGE_LOOP('',(#4141,#4142,#4143,#4144));
#1097=EDGE_LOOP('',(#4145,#4146,#4147,#4148));
#1098=EDGE_LOOP('',(#4149));
#1099=EDGE_LOOP('',(#4150));
#1100=EDGE_LOOP('',(#4151));
#1101=EDGE_LOOP('',(#4152));
#1102=EDGE_LOOP('',(#4153));
#1103=EDGE_LOOP('',(#4154));
#1104=EDGE_LOOP('',(#4155));
#1105=EDGE_LOOP('',(#4156));
#1106=EDGE_LOOP('',(#4157));
#1107=EDGE_LOOP('',(#4158));
#1108=EDGE_LOOP('',(#4159));
#1109=EDGE_LOOP('',(#4160));
#1110=EDGE_LOOP('',(#4161,#4162,#4163,#4164));
#1111=EDGE_LOOP('',(#4165,#4166,#4167,#4168));
#1112=EDGE_LOOP('',(#4169));
#1113=EDGE_LOOP('',(#4170));
#1114=EDGE_LOOP('',(#4171));
#1115=EDGE_LOOP('',(#4172));
#1116=EDGE_LOOP('',(#4173,#4174,#4175,#4176));
#1117=EDGE_LOOP('',(#4177,#4178,#4179,#4180));
#1118=EDGE_LOOP('',(#4181,#4182,#4183,#4184));
#1119=EDGE_LOOP('',(#4185,#4186,#4187,#4188));
#1120=EDGE_LOOP('',(#4189,#4190,#4191,#4192));
#1121=EDGE_LOOP('',(#4193,#4194,#4195,#4196));
#1122=EDGE_LOOP('',(#4197));
#1123=EDGE_LOOP('',(#4198));
#1124=EDGE_LOOP('',(#4199));
#1125=EDGE_LOOP('',(#4200));
#1126=EDGE_LOOP('',(#4201));
#1127=EDGE_LOOP('',(#4202));
#1128=EDGE_LOOP('',(#4203));
#1129=EDGE_LOOP('',(#4204));
#1130=EDGE_LOOP('',(#4205));
#1131=EDGE_LOOP('',(#4206));
#1132=EDGE_LOOP('',(#4207));
#1133=EDGE_LOOP('',(#4208));
#1134=EDGE_LOOP('',(#4209,#4210,#4211,#4212));
#1135=EDGE_LOOP('',(#4213,#4214,#4215,#4216));
#1136=EDGE_LOOP('',(#4217,#4218,#4219,#4220));
#1137=EDGE_LOOP('',(#4221,#4222,#4223,#4224));
#1138=EDGE_LOOP('',(#4225));
#1139=EDGE_LOOP('',(#4226,#4227,#4228,#4229));
#1140=EDGE_LOOP('',(#4230,#4231,#4232,#4233));
#1141=EDGE_LOOP('',(#4234,#4235,#4236,#4237));
#1142=EDGE_LOOP('',(#4238,#4239,#4240,#4241));
#1143=EDGE_LOOP('',(#4242,#4243,#4244,#4245));
#1144=EDGE_LOOP('',(#4246,#4247,#4248,#4249));
#1145=EDGE_LOOP('',(#4250,#4251,#4252,#4253,#4254));
#1146=EDGE_LOOP('',(#4255,#4256,#4257,#4258));
#1147=EDGE_LOOP('',(#4259,#4260,#4261,#4262));
#1148=EDGE_LOOP('',(#4263,#4264,#4265,#4266));
#1149=EDGE_LOOP('',(#4267,#4268,#4269,#4270));
#1150=EDGE_LOOP('',(#4271,#4272,#4273,#4274));
#1151=EDGE_LOOP('',(#4275,#4276,#4277,#4278));
#1152=EDGE_LOOP('',(#4279,#4280,#4281,#4282));
#1153=EDGE_LOOP('',(#4283,#4284,#4285,#4286));
#1154=EDGE_LOOP('',(#4287,#4288,#4289,#4290));
#1155=EDGE_LOOP('',(#4291,#4292,#4293,#4294));
#1156=EDGE_LOOP('',(#4295,#4296,#4297,#4298));
#1157=EDGE_LOOP('',(#4299,#4300,#4301,#4302));
#1158=EDGE_LOOP('',(#4303,#4304,#4305,#4306));
#1159=EDGE_LOOP('',(#4307,#4308,#4309,#4310));
#1160=EDGE_LOOP('',(#4311,#4312,#4313,#4314));
#1161=EDGE_LOOP('',(#4315,#4316,#4317,#4318));
#1162=EDGE_LOOP('',(#4319,#4320,#4321,#4322));
#1163=EDGE_LOOP('',(#4323,#4324,#4325,#4326));
#1164=EDGE_LOOP('',(#4327,#4328,#4329,#4330));
#1165=EDGE_LOOP('',(#4331,#4332,#4333,#4334));
#1166=EDGE_LOOP('',(#4335,#4336,#4337,#4338));
#1167=EDGE_LOOP('',(#4339,#4340,#4341,#4342));
#1168=EDGE_LOOP('',(#4343,#4344,#4345,#4346));
#1169=EDGE_LOOP('',(#4347,#4348,#4349,#4350));
#1170=EDGE_LOOP('',(#4351,#4352,#4353,#4354));
#1171=EDGE_LOOP('',(#4355,#4356,#4357,#4358));
#1172=EDGE_LOOP('',(#4359,#4360,#4361,#4362));
#1173=EDGE_LOOP('',(#4363,#4364,#4365,#4366));
#1174=EDGE_LOOP('',(#4367,#4368,#4369,#4370));
#1175=EDGE_LOOP('',(#4371,#4372,#4373,#4374));
#1176=EDGE_LOOP('',(#4375,#4376,#4377,#4378));
#1177=EDGE_LOOP('',(#4379));
#1178=EDGE_LOOP('',(#4380));
#1179=EDGE_LOOP('',(#4381,#4382,#4383,#4384,#4385,#4386,#4387,#4388));
#1180=EDGE_LOOP('',(#4389,#4390,#4391,#4392));
#1181=EDGE_LOOP('',(#4393));
#1182=EDGE_LOOP('',(#4394));
#1183=EDGE_LOOP('',(#4395,#4396,#4397,#4398));
#1184=EDGE_LOOP('',(#4399,#4400,#4401,#4402));
#1185=EDGE_LOOP('',(#4403));
#1186=EDGE_LOOP('',(#4404));
#1187=EDGE_LOOP('',(#4405));
#1188=EDGE_LOOP('',(#4406));
#1189=EDGE_LOOP('',(#4407,#4408,#4409,#4410));
#1190=EDGE_LOOP('',(#4411,#4412,#4413,#4414));
#1191=EDGE_LOOP('',(#4415,#4416,#4417,#4418));
#1192=EDGE_LOOP('',(#4419,#4420,#4421,#4422));
#1193=EDGE_LOOP('',(#4423,#4424,#4425,#4426));
#1194=EDGE_LOOP('',(#4427,#4428,#4429,#4430));
#1195=EDGE_LOOP('',(#4431,#4432,#4433,#4434));
#1196=EDGE_LOOP('',(#4435,#4436,#4437,#4438));
#1197=EDGE_LOOP('',(#4439,#4440,#4441,#4442));
#1198=EDGE_LOOP('',(#4443,#4444,#4445,#4446));
#1199=EDGE_LOOP('',(#4447,#4448,#4449,#4450));
#1200=EDGE_LOOP('',(#4451,#4452,#4453,#4454));
#1201=EDGE_LOOP('',(#4455,#4456,#4457,#4458));
#1202=EDGE_LOOP('',(#4459,#4460,#4461,#4462));
#1203=EDGE_LOOP('',(#4463,#4464,#4465,#4466));
#1204=EDGE_LOOP('',(#4467,#4468,#4469,#4470));
#1205=EDGE_LOOP('',(#4471,#4472,#4473,#4474));
#1206=EDGE_LOOP('',(#4475,#4476,#4477,#4478));
#1207=EDGE_LOOP('',(#4479,#4480,#4481,#4482));
#1208=EDGE_LOOP('',(#4483,#4484,#4485,#4486));
#1209=EDGE_LOOP('',(#4487,#4488,#4489,#4490));
#1210=EDGE_LOOP('',(#4491,#4492,#4493,#4494));
#1211=EDGE_LOOP('',(#4495,#4496,#4497,#4498));
#1212=EDGE_LOOP('',(#4499,#4500,#4501,#4502));
#1213=EDGE_LOOP('',(#4503,#4504,#4505,#4506));
#1214=EDGE_LOOP('',(#4507,#4508,#4509,#4510));
#1215=EDGE_LOOP('',(#4511,#4512,#4513,#4514));
#1216=EDGE_LOOP('',(#4515,#4516,#4517,#4518));
#1217=EDGE_LOOP('',(#4519,#4520,#4521,#4522));
#1218=EDGE_LOOP('',(#4523,#4524,#4525,#4526));
#1219=EDGE_LOOP('',(#4527,#4528,#4529,#4530));
#1220=EDGE_LOOP('',(#4531,#4532,#4533,#4534));
#1221=EDGE_LOOP('',(#4535,#4536,#4537,#4538));
#1222=EDGE_LOOP('',(#4539,#4540,#4541,#4542));
#1223=EDGE_LOOP('',(#4543,#4544,#4545,#4546));
#1224=EDGE_LOOP('',(#4547,#4548,#4549,#4550));
#1225=EDGE_LOOP('',(#4551,#4552,#4553,#4554));
#1226=EDGE_LOOP('',(#4555,#4556,#4557,#4558));
#1227=EDGE_LOOP('',(#4559,#4560,#4561,#4562));
#1228=EDGE_LOOP('',(#4563,#4564,#4565,#4566));
#1229=EDGE_LOOP('',(#4567,#4568,#4569,#4570));
#1230=EDGE_LOOP('',(#4571,#4572,#4573,#4574));
#1231=EDGE_LOOP('',(#4575,#4576,#4577,#4578));
#1232=EDGE_LOOP('',(#4579,#4580,#4581,#4582));
#1233=EDGE_LOOP('',(#4583,#4584,#4585,#4586));
#1234=EDGE_LOOP('',(#4587,#4588,#4589,#4590));
#1235=EDGE_LOOP('',(#4591,#4592,#4593,#4594));
#1236=EDGE_LOOP('',(#4595,#4596,#4597,#4598));
#1237=EDGE_LOOP('',(#4599,#4600,#4601,#4602));
#1238=EDGE_LOOP('',(#4603,#4604,#4605,#4606));
#1239=EDGE_LOOP('',(#4607,#4608,#4609,#4610));
#1240=EDGE_LOOP('',(#4611,#4612,#4613,#4614));
#1241=EDGE_LOOP('',(#4615,#4616,#4617,#4618));
#1242=EDGE_LOOP('',(#4619,#4620,#4621,#4622));
#1243=EDGE_LOOP('',(#4623,#4624,#4625,#4626));
#1244=EDGE_LOOP('',(#4627,#4628,#4629,#4630));
#1245=EDGE_LOOP('',(#4631,#4632,#4633,#4634));
#1246=EDGE_LOOP('',(#4635,#4636,#4637,#4638));
#1247=EDGE_LOOP('',(#4639,#4640,#4641,#4642));
#1248=EDGE_LOOP('',(#4643,#4644,#4645,#4646));
#1249=EDGE_LOOP('',(#4647,#4648,#4649,#4650));
#1250=EDGE_LOOP('',(#4651,#4652,#4653,#4654));
#1251=EDGE_LOOP('',(#4655,#4656,#4657,#4658));
#1252=EDGE_LOOP('',(#4659,#4660,#4661,#4662));
#1253=EDGE_LOOP('',(#4663,#4664,#4665,#4666));
#1254=EDGE_LOOP('',(#4667,#4668,#4669,#4670));
#1255=EDGE_LOOP('',(#4671));
#1256=EDGE_LOOP('',(#4672));
#1257=EDGE_LOOP('',(#4673));
#1258=EDGE_LOOP('',(#4674,#4675,#4676,#4677,#4678));
#1259=EDGE_LOOP('',(#4679,#4680,#4681,#4682));
#1260=EDGE_LOOP('',(#4683,#4684,#4685,#4686));
#1261=EDGE_LOOP('',(#4687));
#1262=EDGE_LOOP('',(#4688,#4689,#4690,#4691));
#1263=EDGE_LOOP('',(#4692,#4693,#4694,#4695,#4696,#4697,#4698,#4699,#4700,
#4701,#4702,#4703,#4704,#4705,#4706,#4707,#4708,#4709,#4710,#4711));
#1264=EDGE_LOOP('',(#4712,#4713,#4714,#4715,#4716,#4717,#4718,#4719,#4720,
#4721,#4722,#4723,#4724,#4725,#4726,#4727,#4728,#4729,#4730,#4731));
#1265=EDGE_LOOP('',(#4732));
#1266=EDGE_LOOP('',(#4733));
#1267=EDGE_LOOP('',(#4734,#4735,#4736,#4737));
#1268=EDGE_LOOP('',(#4738,#4739,#4740,#4741));
#1269=EDGE_LOOP('',(#4742,#4743,#4744,#4745));
#1270=EDGE_LOOP('',(#4746,#4747,#4748,#4749));
#1271=EDGE_LOOP('',(#4750,#4751,#4752,#4753));
#1272=EDGE_LOOP('',(#4754,#4755,#4756,#4757,#4758,#4759,#4760,#4761,#4762,
#4763,#4764,#4765,#4766,#4767,#4768,#4769,#4770,#4771,#4772,#4773));
#1273=EDGE_LOOP('',(#4774,#4775,#4776,#4777,#4778,#4779,#4780,#4781,#4782,
#4783,#4784,#4785,#4786,#4787,#4788,#4789,#4790,#4791,#4792,#4793));
#1274=EDGE_LOOP('',(#4794,#4795,#4796,#4797));
#1275=EDGE_LOOP('',(#4798,#4799,#4800,#4801,#4802,#4803,#4804,#4805,#4806,
#4807,#4808,#4809,#4810,#4811,#4812,#4813,#4814,#4815,#4816,#4817));
#1276=EDGE_LOOP('',(#4818,#4819,#4820,#4821,#4822,#4823,#4824,#4825,#4826,
#4827,#4828,#4829,#4830,#4831,#4832,#4833,#4834,#4835,#4836,#4837));
#1277=EDGE_LOOP('',(#4838,#4839,#4840,#4841));
#1278=EDGE_LOOP('',(#4842,#4843,#4844,#4845,#4846,#4847,#4848,#4849,#4850,
#4851,#4852,#4853,#4854,#4855,#4856,#4857,#4858,#4859,#4860,#4861));
#1279=EDGE_LOOP('',(#4862,#4863,#4864,#4865,#4866,#4867,#4868,#4869,#4870,
#4871,#4872,#4873,#4874,#4875,#4876,#4877,#4878,#4879,#4880,#4881));
#1280=EDGE_LOOP('',(#4882,#4883,#4884,#4885));
#1281=EDGE_LOOP('',(#4886,#4887,#4888,#4889));
#1282=EDGE_LOOP('',(#4890,#4891,#4892,#4893));
#1283=EDGE_LOOP('',(#4894,#4895,#4896,#4897));
#1284=EDGE_LOOP('',(#4898,#4899,#4900,#4901));
#1285=EDGE_LOOP('',(#4902,#4903,#4904,#4905));
#1286=EDGE_LOOP('',(#4906,#4907,#4908,#4909));
#1287=EDGE_LOOP('',(#4910,#4911,#4912,#4913));
#1288=EDGE_LOOP('',(#4914));
#1289=EDGE_LOOP('',(#4915));
#1290=EDGE_LOOP('',(#4916));
#1291=EDGE_LOOP('',(#4917));
#1292=EDGE_LOOP('',(#4918));
#1293=EDGE_LOOP('',(#4919));
#1294=EDGE_LOOP('',(#4920,#4921,#4922,#4923));
#1295=EDGE_LOOP('',(#4924));
#1296=EDGE_LOOP('',(#4925));
#1297=EDGE_LOOP('',(#4926));
#1298=EDGE_LOOP('',(#4927));
#1299=EDGE_LOOP('',(#4928));
#1300=EDGE_LOOP('',(#4929));
#1301=EDGE_LOOP('',(#4930,#4931,#4932,#4933));
#1302=EDGE_LOOP('',(#4934,#4935,#4936,#4937));
#1303=EDGE_LOOP('',(#4938,#4939,#4940,#4941));
#1304=EDGE_LOOP('',(#4942,#4943,#4944,#4945));
#1305=EDGE_LOOP('',(#4946,#4947,#4948,#4949));
#1306=EDGE_LOOP('',(#4950,#4951,#4952,#4953,#4954,#4955,#4956,#4957,#4958,
#4959,#4960,#4961,#4962,#4963,#4964,#4965));
#1307=EDGE_LOOP('',(#4966,#4967,#4968,#4969,#4970,#4971,#4972,#4973,#4974,
#4975,#4976,#4977));
#1308=EDGE_LOOP('',(#4978));
#1309=EDGE_LOOP('',(#4979,#4980,#4981,#4982));
#1310=EDGE_LOOP('',(#4983,#4984,#4985,#4986));
#1311=EDGE_LOOP('',(#4987,#4988,#4989,#4990));
#1312=EDGE_LOOP('',(#4991,#4992,#4993,#4994));
#1313=EDGE_LOOP('',(#4995,#4996,#4997,#4998));
#1314=EDGE_LOOP('',(#4999));
#1315=EDGE_LOOP('',(#5000,#5001,#5002,#5003));
#1316=EDGE_LOOP('',(#5004,#5005,#5006,#5007));
#1317=EDGE_LOOP('',(#5008,#5009,#5010,#5011));
#1318=EDGE_LOOP('',(#5012,#5013,#5014,#5015));
#1319=EDGE_LOOP('',(#5016));
#1320=EDGE_LOOP('',(#5017,#5018,#5019,#5020));
#1321=EDGE_LOOP('',(#5021,#5022,#5023,#5024));
#1322=EDGE_LOOP('',(#5025,#5026,#5027,#5028));
#1323=EDGE_LOOP('',(#5029));
#1324=EDGE_LOOP('',(#5030));
#1325=EDGE_LOOP('',(#5031));
#1326=EDGE_LOOP('',(#5032));
#1327=EDGE_LOOP('',(#5033));
#1328=EDGE_LOOP('',(#5034));
#1329=EDGE_LOOP('',(#5035,#5036,#5037,#5038));
#1330=EDGE_LOOP('',(#5039,#5040,#5041,#5042));
#1331=EDGE_LOOP('',(#5043,#5044,#5045,#5046));
#1332=EDGE_LOOP('',(#5047,#5048,#5049,#5050));
#1333=EDGE_LOOP('',(#5051));
#1334=EDGE_LOOP('',(#5052));
#1335=EDGE_LOOP('',(#5053));
#1336=EDGE_LOOP('',(#5054));
#1337=EDGE_LOOP('',(#5055));
#1338=EDGE_LOOP('',(#5056));
#1339=EDGE_LOOP('',(#5057,#5058,#5059,#5060));
#1340=EDGE_LOOP('',(#5061,#5062));
#1341=EDGE_LOOP('',(#5063));
#1342=EDGE_LOOP('',(#5064,#5065,#5066,#5067));
#1343=EDGE_LOOP('',(#5068,#5069,#5070,#5071,#5072));
#1344=EDGE_LOOP('',(#5073,#5074,#5075,#5076));
#1345=EDGE_LOOP('',(#5077,#5078,#5079,#5080,#5081,#5082));
#1346=EDGE_LOOP('',(#5083,#5084,#5085,#5086));
#1347=EDGE_LOOP('',(#5087,#5088));
#1348=EDGE_LOOP('',(#5089,#5090,#5091,#5092));
#1349=EDGE_LOOP('',(#5093,#5094,#5095,#5096));
#1350=EDGE_LOOP('',(#5097,#5098,#5099,#5100));
#1351=EDGE_LOOP('',(#5101,#5102,#5103,#5104));
#1352=EDGE_LOOP('',(#5105,#5106,#5107,#5108));
#1353=EDGE_LOOP('',(#5109));
#1354=EDGE_LOOP('',(#5110));
#1355=EDGE_LOOP('',(#5111));
#1356=EDGE_LOOP('',(#5112));
#1357=EDGE_LOOP('',(#5113,#5114,#5115,#5116));
#1358=EDGE_LOOP('',(#5117,#5118,#5119,#5120));
#1359=EDGE_LOOP('',(#5121));
#1360=EDGE_LOOP('',(#5122));
#1361=EDGE_LOOP('',(#5123,#5124,#5125,#5126,#5127));
#1362=EDGE_LOOP('',(#5128));
#1363=EDGE_LOOP('',(#5129,#5130,#5131,#5132));
#1364=EDGE_LOOP('',(#5133));
#1365=EDGE_LOOP('',(#5134));
#1366=EDGE_LOOP('',(#5135));
#1367=EDGE_LOOP('',(#5136));
#1368=EDGE_LOOP('',(#5137));
#1369=EDGE_LOOP('',(#5138));
#1370=EDGE_LOOP('',(#5139));
#1371=EDGE_LOOP('',(#5140));
#1372=EDGE_LOOP('',(#5141));
#1373=EDGE_LOOP('',(#5142));
#1374=EDGE_LOOP('',(#5143));
#1375=EDGE_LOOP('',(#5144));
#1376=EDGE_LOOP('',(#5145,#5146,#5147,#5148));
#1377=EDGE_LOOP('',(#5149,#5150,#5151,#5152));
#1378=EDGE_LOOP('',(#5153,#5154,#5155,#5156));
#1379=EDGE_LOOP('',(#5157,#5158,#5159,#5160));
#1380=EDGE_LOOP('',(#5161,#5162,#5163,#5164));
#1381=EDGE_LOOP('',(#5165,#5166,#5167,#5168,#5169));
#1382=EDGE_LOOP('',(#5170,#5171,#5172,#5173,#5174,#5175,#5176,#5177,#5178,
#5179));
#1383=EDGE_LOOP('',(#5180,#5181,#5182,#5183));
#1384=EDGE_LOOP('',(#5184,#5185,#5186,#5187));
#1385=EDGE_LOOP('',(#5188,#5189,#5190,#5191));
#1386=EDGE_LOOP('',(#5192,#5193,#5194,#5195));
#1387=EDGE_LOOP('',(#5196,#5197,#5198,#5199));
#1388=EDGE_LOOP('',(#5200,#5201,#5202,#5203));
#1389=EDGE_LOOP('',(#5204,#5205,#5206,#5207));
#1390=EDGE_LOOP('',(#5208,#5209,#5210,#5211));
#1391=EDGE_LOOP('',(#5212,#5213,#5214,#5215));
#1392=EDGE_LOOP('',(#5216,#5217,#5218,#5219));
#1393=EDGE_LOOP('',(#5220,#5221,#5222,#5223));
#1394=EDGE_LOOP('',(#5224));
#1395=EDGE_LOOP('',(#5225));
#1396=EDGE_LOOP('',(#5226));
#1397=EDGE_LOOP('',(#5227));
#1398=EDGE_LOOP('',(#5228));
#1399=EDGE_LOOP('',(#5229));
#1400=EDGE_LOOP('',(#5230));
#1401=EDGE_LOOP('',(#5231));
#1402=EDGE_LOOP('',(#5232,#5233,#5234,#5235));
#1403=EDGE_LOOP('',(#5236,#5237,#5238,#5239));
#1404=EDGE_LOOP('',(#5240,#5241,#5242,#5243));
#1405=EDGE_LOOP('',(#5244,#5245,#5246,#5247));
#1406=EDGE_LOOP('',(#5248,#5249,#5250,#5251));
#1407=EDGE_LOOP('',(#5252,#5253,#5254,#5255));
#1408=EDGE_LOOP('',(#5256));
#1409=EDGE_LOOP('',(#5257,#5258,#5259,#5260));
#1410=EDGE_LOOP('',(#5261,#5262,#5263,#5264));
#1411=EDGE_LOOP('',(#5265));
#1412=EDGE_LOOP('',(#5266));
#1413=EDGE_LOOP('',(#5267));
#1414=EDGE_LOOP('',(#5268));
#1415=EDGE_LOOP('',(#5269,#5270,#5271,#5272));
#1416=EDGE_LOOP('',(#5273,#5274,#5275,#5276));
#1417=EDGE_LOOP('',(#5277));
#1418=EDGE_LOOP('',(#5278));
#1419=EDGE_LOOP('',(#5279));
#1420=EDGE_LOOP('',(#5280));
#1421=EDGE_LOOP('',(#5281,#5282,#5283,#5284));
#1422=EDGE_LOOP('',(#5285,#5286,#5287,#5288));
#1423=EDGE_LOOP('',(#5289));
#1424=EDGE_LOOP('',(#5290));
#1425=EDGE_LOOP('',(#5291));
#1426=EDGE_LOOP('',(#5292));
#1427=EDGE_LOOP('',(#5293,#5294,#5295,#5296));
#1428=EDGE_LOOP('',(#5297,#5298,#5299,#5300));
#1429=EDGE_LOOP('',(#5301));
#1430=EDGE_LOOP('',(#5302));
#1431=EDGE_LOOP('',(#5303));
#1432=EDGE_LOOP('',(#5304));
#1433=EDGE_LOOP('',(#5305,#5306,#5307,#5308));
#1434=EDGE_LOOP('',(#5309,#5310,#5311,#5312));
#1435=EDGE_LOOP('',(#5313,#5314,#5315,#5316));
#1436=EDGE_LOOP('',(#5317,#5318,#5319,#5320));
#1437=EDGE_LOOP('',(#5321,#5322,#5323,#5324));
#1438=EDGE_LOOP('',(#5325,#5326,#5327,#5328));
#1439=EDGE_LOOP('',(#5329,#5330,#5331,#5332));
#1440=EDGE_LOOP('',(#5333,#5334,#5335,#5336));
#1441=EDGE_LOOP('',(#5337));
#1442=EDGE_LOOP('',(#5338));
#1443=EDGE_LOOP('',(#5339));
#1444=EDGE_LOOP('',(#5340));
#1445=EDGE_LOOP('',(#5341,#5342,#5343,#5344));
#1446=EDGE_LOOP('',(#5345,#5346,#5347,#5348));
#1447=EDGE_LOOP('',(#5349));
#1448=EDGE_LOOP('',(#5350));
#1449=EDGE_LOOP('',(#5351));
#1450=EDGE_LOOP('',(#5352));
#1451=EDGE_LOOP('',(#5353,#5354,#5355,#5356));
#1452=EDGE_LOOP('',(#5357,#5358,#5359,#5360));
#1453=EDGE_LOOP('',(#5361));
#1454=EDGE_LOOP('',(#5362));
#1455=EDGE_LOOP('',(#5363));
#1456=EDGE_LOOP('',(#5364));
#1457=EDGE_LOOP('',(#5365,#5366,#5367,#5368));
#1458=EDGE_LOOP('',(#5369,#5370,#5371,#5372));
#1459=EDGE_LOOP('',(#5373));
#1460=EDGE_LOOP('',(#5374));
#1461=EDGE_LOOP('',(#5375));
#1462=EDGE_LOOP('',(#5376));
#1463=EDGE_LOOP('',(#5377,#5378,#5379,#5380));
#1464=EDGE_LOOP('',(#5381,#5382,#5383,#5384));
#1465=EDGE_LOOP('',(#5385,#5386,#5387,#5388));
#1466=EDGE_LOOP('',(#5389,#5390,#5391,#5392));
#1467=EDGE_LOOP('',(#5393,#5394,#5395,#5396));
#1468=EDGE_LOOP('',(#5397,#5398,#5399,#5400));
#1469=EDGE_LOOP('',(#5401,#5402,#5403,#5404,#5405,#5406,#5407,#5408));
#1470=EDGE_LOOP('',(#5409,#5410,#5411,#5412));
#1471=EDGE_LOOP('',(#5413,#5414,#5415,#5416));
#1472=EDGE_LOOP('',(#5417,#5418,#5419,#5420));
#1473=EDGE_LOOP('',(#5421,#5422,#5423,#5424));
#1474=EDGE_LOOP('',(#5425,#5426,#5427,#5428));
#1475=EDGE_LOOP('',(#5429,#5430,#5431,#5432));
#1476=EDGE_LOOP('',(#5433,#5434,#5435,#5436));
#1477=EDGE_LOOP('',(#5437,#5438,#5439,#5440));
#1478=EDGE_LOOP('',(#5441,#5442,#5443,#5444));
#1479=EDGE_LOOP('',(#5445,#5446,#5447,#5448));
#1480=EDGE_LOOP('',(#5449,#5450,#5451,#5452));
#1481=EDGE_LOOP('',(#5453,#5454,#5455,#5456));
#1482=EDGE_LOOP('',(#5457,#5458,#5459,#5460));
#1483=EDGE_LOOP('',(#5461,#5462,#5463,#5464,#5465,#5466,#5467,#5468));
#1484=EDGE_LOOP('',(#5469,#5470,#5471,#5472,#5473,#5474,#5475,#5476,#5477,
#5478,#5479,#5480,#5481,#5482,#5483,#5484,#5485,#5486));
#1485=EDGE_LOOP('',(#5487,#5488,#5489,#5490));
#1486=EDGE_LOOP('',(#5491,#5492,#5493,#5494,#5495,#5496,#5497,#5498,#5499,
#5500,#5501,#5502,#5503,#5504,#5505,#5506,#5507,#5508,#5509));
#1487=EDGE_LOOP('',(#5510,#5511,#5512,#5513,#5514));
#1488=EDGE_LOOP('',(#5515,#5516,#5517,#5518));
#1489=EDGE_LOOP('',(#5519,#5520,#5521,#5522));
#1490=EDGE_LOOP('',(#5523,#5524,#5525,#5526));
#1491=EDGE_LOOP('',(#5527,#5528,#5529,#5530));
#1492=EDGE_LOOP('',(#5531,#5532,#5533,#5534));
#1493=EDGE_LOOP('',(#5535,#5536,#5537,#5538));
#1494=EDGE_LOOP('',(#5539,#5540,#5541,#5542));
#1495=EDGE_LOOP('',(#5543,#5544,#5545,#5546,#5547,#5548));
#1496=EDGE_LOOP('',(#5549));
#1497=EDGE_LOOP('',(#5550));
#1498=EDGE_LOOP('',(#5551,#5552,#5553,#5554));
#1499=EDGE_LOOP('',(#5555));
#1500=EDGE_LOOP('',(#5556,#5557,#5558,#5559,#5560,#5561));
#1501=EDGE_LOOP('',(#5562));
#1502=LINE('',#8657,#1871);
#1503=LINE('',#8663,#1872);
#1504=LINE('',#8673,#1873);
#1505=LINE('',#8679,#1874);
#1506=LINE('',#8685,#1875);
#1507=LINE('',#8691,#1876);
#1508=LINE('',#8696,#1877);
#1509=LINE('',#8698,#1878);
#1510=LINE('',#8700,#1879);
#1511=LINE('',#8701,#1880);
#1512=LINE('',#8707,#1881);
#1513=LINE('',#8710,#1882);
#1514=LINE('',#8712,#1883);
#1515=LINE('',#8713,#1884);
#1516=LINE('',#8721,#1885);
#1517=LINE('',#8723,#1886);
#1518=LINE('',#8725,#1887);
#1519=LINE('',#8726,#1888);
#1520=LINE('',#8732,#1889);
#1521=LINE('',#8735,#1890);
#1522=LINE('',#8737,#1891);
#1523=LINE('',#8738,#1892);
#1524=LINE('',#8746,#1893);
#1525=LINE('',#8748,#1894);
#1526=LINE('',#8750,#1895);
#1527=LINE('',#8751,#1896);
#1528=LINE('',#8757,#1897);
#1529=LINE('',#8760,#1898);
#1530=LINE('',#8762,#1899);
#1531=LINE('',#8763,#1900);
#1532=LINE('',#8771,#1901);
#1533=LINE('',#8773,#1902);
#1534=LINE('',#8775,#1903);
#1535=LINE('',#8776,#1904);
#1536=LINE('',#8782,#1905);
#1537=LINE('',#8785,#1906);
#1538=LINE('',#8787,#1907);
#1539=LINE('',#8788,#1908);
#1540=LINE('',#8796,#1909);
#1541=LINE('',#8798,#1910);
#1542=LINE('',#8800,#1911);
#1543=LINE('',#8801,#1912);
#1544=LINE('',#8807,#1913);
#1545=LINE('',#8810,#1914);
#1546=LINE('',#8812,#1915);
#1547=LINE('',#8813,#1916);
#1548=LINE('',#8821,#1917);
#1549=LINE('',#8823,#1918);
#1550=LINE('',#8825,#1919);
#1551=LINE('',#8826,#1920);
#1552=LINE('',#8832,#1921);
#1553=LINE('',#8835,#1922);
#1554=LINE('',#8837,#1923);
#1555=LINE('',#8838,#1924);
#1556=LINE('',#8846,#1925);
#1557=LINE('',#8848,#1926);
#1558=LINE('',#8850,#1927);
#1559=LINE('',#8851,#1928);
#1560=LINE('',#8855,#1929);
#1561=LINE('',#8857,#1930);
#1562=LINE('',#8859,#1931);
#1563=LINE('',#8860,#1932);
#1564=LINE('',#8864,#1933);
#1565=LINE('',#8866,#1934);
#1566=LINE('',#8868,#1935);
#1567=LINE('',#8869,#1936);
#1568=LINE('',#8873,#1937);
#1569=LINE('',#8875,#1938);
#1570=LINE('',#8877,#1939);
#1571=LINE('',#8878,#1940);
#1572=LINE('',#8885,#1941);
#1573=LINE('',#8889,#1942);
#1574=LINE('',#8897,#1943);
#1575=LINE('',#8902,#1944);
#1576=LINE('',#8907,#1945);
#1577=LINE('',#8910,#1946);
#1578=LINE('',#8913,#1947);
#1579=LINE('',#8917,#1948);
#1580=LINE('',#8919,#1949);
#1581=LINE('',#8922,#1950);
#1582=LINE('',#8928,#1951);
#1583=LINE('',#8937,#1952);
#1584=LINE('',#8943,#1953);
#1585=LINE('',#8953,#1954);
#1586=LINE('',#8959,#1955);
#1587=LINE('',#8965,#1956);
#1588=LINE('',#8971,#1957);
#1589=LINE('',#8975,#1958);
#1590=LINE('',#8981,#1959);
#1591=LINE('',#8989,#1960);
#1592=LINE('',#8991,#1961);
#1593=LINE('',#8993,#1962);
#1594=LINE('',#8994,#1963);
#1595=LINE('',#8997,#1964);
#1596=LINE('',#8999,#1965);
#1597=LINE('',#9000,#1966);
#1598=LINE('',#9004,#1967);
#1599=LINE('',#9005,#1968);
#1600=LINE('',#9006,#1969);
#1601=LINE('',#9016,#1970);
#1602=LINE('',#9019,#1971);
#1603=LINE('',#9024,#1972);
#1604=LINE('',#9027,#1973);
#1605=LINE('',#9032,#1974);
#1606=LINE('',#9035,#1975);
#1607=LINE('',#9040,#1976);
#1608=LINE('',#9043,#1977);
#1609=LINE('',#9048,#1978);
#1610=LINE('',#9051,#1979);
#1611=LINE('',#9056,#1980);
#1612=LINE('',#9059,#1981);
#1613=LINE('',#9067,#1982);
#1614=LINE('',#9068,#1983);
#1615=LINE('',#9071,#1984);
#1616=LINE('',#9072,#1985);
#1617=LINE('',#9076,#1986);
#1618=LINE('',#9078,#1987);
#1619=LINE('',#9084,#1988);
#1620=LINE('',#9085,#1989);
#1621=LINE('',#9088,#1990);
#1622=LINE('',#9089,#1991);
#1623=LINE('',#9093,#1992);
#1624=LINE('',#9095,#1993);
#1625=LINE('',#9101,#1994);
#1626=LINE('',#9102,#1995);
#1627=LINE('',#9105,#1996);
#1628=LINE('',#9106,#1997);
#1629=LINE('',#9110,#1998);
#1630=LINE('',#9112,#1999);
#1631=LINE('',#9118,#2000);
#1632=LINE('',#9119,#2001);
#1633=LINE('',#9122,#2002);
#1634=LINE('',#9123,#2003);
#1635=LINE('',#9127,#2004);
#1636=LINE('',#9129,#2005);
#1637=LINE('',#9135,#2006);
#1638=LINE('',#9136,#2007);
#1639=LINE('',#9139,#2008);
#1640=LINE('',#9140,#2009);
#1641=LINE('',#9144,#2010);
#1642=LINE('',#9146,#2011);
#1643=LINE('',#9152,#2012);
#1644=LINE('',#9153,#2013);
#1645=LINE('',#9156,#2014);
#1646=LINE('',#9157,#2015);
#1647=LINE('',#9161,#2016);
#1648=LINE('',#9163,#2017);
#1649=LINE('',#9169,#2018);
#1650=LINE('',#9175,#2019);
#1651=LINE('',#9179,#2020);
#1652=LINE('',#9186,#2021);
#1653=LINE('',#9192,#2022);
#1654=LINE('',#9200,#2023);
#1655=LINE('',#9221,#2024);
#1656=LINE('',#9272,#2025);
#1657=LINE('',#9323,#2026);
#1658=LINE('',#9371,#2027);
#1659=LINE('',#9422,#2028);
#1660=LINE('',#9473,#2029);
#1661=LINE('',#9521,#2030);
#1662=LINE('',#9560,#2031);
#1663=LINE('',#9581,#2032);
#1664=LINE('',#9632,#2033);
#1665=LINE('',#9683,#2034);
#1666=LINE('',#9731,#2035);
#1667=LINE('',#9782,#2036);
#1668=LINE('',#9833,#2037);
#1669=LINE('',#9881,#2038);
#1670=LINE('',#9920,#2039);
#1671=LINE('',#9941,#2040);
#1672=LINE('',#9992,#2041);
#1673=LINE('',#10043,#2042);
#1674=LINE('',#10091,#2043);
#1675=LINE('',#10142,#2044);
#1676=LINE('',#10193,#2045);
#1677=LINE('',#10241,#2046);
#1678=LINE('',#10280,#2047);
#1679=LINE('',#10301,#2048);
#1680=LINE('',#10352,#2049);
#1681=LINE('',#10403,#2050);
#1682=LINE('',#10451,#2051);
#1683=LINE('',#10502,#2052);
#1684=LINE('',#10553,#2053);
#1685=LINE('',#10601,#2054);
#1686=LINE('',#10640,#2055);
#1687=LINE('',#10664,#2056);
#1688=LINE('',#10688,#2057);
#1689=LINE('',#10713,#2058);
#1690=LINE('',#10738,#2059);
#1691=LINE('',#10762,#2060);
#1692=LINE('',#10787,#2061);
#1693=LINE('',#10812,#2062);
#1694=LINE('',#10829,#2063);
#1695=LINE('',#10853,#2064);
#1696=LINE('',#10877,#2065);
#1697=LINE('',#10902,#2066);
#1698=LINE('',#10927,#2067);
#1699=LINE('',#10951,#2068);
#1700=LINE('',#10976,#2069);
#1701=LINE('',#11001,#2070);
#1702=LINE('',#11018,#2071);
#1703=LINE('',#11042,#2072);
#1704=LINE('',#11066,#2073);
#1705=LINE('',#11091,#2074);
#1706=LINE('',#11116,#2075);
#1707=LINE('',#11140,#2076);
#1708=LINE('',#11165,#2077);
#1709=LINE('',#11190,#2078);
#1710=LINE('',#11207,#2079);
#1711=LINE('',#11231,#2080);
#1712=LINE('',#11255,#2081);
#1713=LINE('',#11280,#2082);
#1714=LINE('',#11305,#2083);
#1715=LINE('',#11329,#2084);
#1716=LINE('',#11354,#2085);
#1717=LINE('',#11379,#2086);
#1718=LINE('',#11397,#2087);
#1719=LINE('',#11403,#2088);
#1720=LINE('',#11413,#2089);
#1721=LINE('',#11416,#2090);
#1722=LINE('',#11421,#2091);
#1723=LINE('',#11424,#2092);
#1724=LINE('',#11427,#2093);
#1725=LINE('',#11431,#2094);
#1726=LINE('',#14456,#2095);
#1727=LINE('',#14462,#2096);
#1728=LINE('',#14468,#2097);
#1729=LINE('',#14474,#2098);
#1730=LINE('',#14483,#2099);
#1731=LINE('',#14489,#2100);
#1732=LINE('',#14492,#2101);
#1733=LINE('',#14494,#2102);
#1734=LINE('',#14495,#2103);
#1735=LINE('',#14498,#2104);
#1736=LINE('',#14500,#2105);
#1737=LINE('',#14501,#2106);
#1738=LINE('',#14504,#2107);
#1739=LINE('',#14506,#2108);
#1740=LINE('',#14507,#2109);
#1741=LINE('',#14510,#2110);
#1742=LINE('',#14512,#2111);
#1743=LINE('',#14513,#2112);
#1744=LINE('',#14516,#2113);
#1745=LINE('',#14519,#2114);
#1746=LINE('',#14521,#2115);
#1747=LINE('',#14525,#2116);
#1748=LINE('',#14530,#2117);
#1749=LINE('',#14534,#2118);
#1750=LINE('',#14537,#2119);
#1751=LINE('',#14539,#2120);
#1752=LINE('',#14546,#2121);
#1753=LINE('',#14648,#2122);
#1754=LINE('',#14652,#2123);
#1755=LINE('',#14656,#2124);
#1756=LINE('',#14660,#2125);
#1757=LINE('',#14668,#2126);
#1758=LINE('',#14672,#2127);
#1759=LINE('',#14677,#2128);
#1760=LINE('',#14680,#2129);
#1761=LINE('',#14752,#2130);
#1762=LINE('',#14754,#2131);
#1763=LINE('',#14814,#2132);
#1764=LINE('',#14821,#2133);
#1765=LINE('',#14827,#2134);
#1766=LINE('',#14833,#2135);
#1767=LINE('',#14839,#2136);
#1768=LINE('',#14845,#2137);
#1769=LINE('',#14851,#2138);
#1770=LINE('',#14863,#2139);
#1771=LINE('',#14868,#2140);
#1772=LINE('',#14874,#2141);
#1773=LINE('',#14881,#2142);
#1774=LINE('',#14885,#2143);
#1775=LINE('',#14909,#2144);
#1776=LINE('',#14911,#2145);
#1777=LINE('',#14914,#2146);
#1778=LINE('',#14916,#2147);
#1779=LINE('',#14917,#2148);
#1780=LINE('',#14940,#2149);
#1781=LINE('',#14942,#2150);
#1782=LINE('',#14943,#2151);
#1783=LINE('',#14950,#2152);
#1784=LINE('',#14955,#2153);
#1785=LINE('',#14957,#2154);
#1786=LINE('',#14959,#2155);
#1787=LINE('',#14960,#2156);
#1788=LINE('',#14983,#2157);
#1789=LINE('',#14986,#2158);
#1790=LINE('',#14988,#2159);
#1791=LINE('',#14989,#2160);
#1792=LINE('',#15014,#2161);
#1793=LINE('',#15016,#2162);
#1794=LINE('',#15018,#2163);
#1795=LINE('',#15019,#2164);
#1796=LINE('',#15042,#2165);
#1797=LINE('',#15045,#2166);
#1798=LINE('',#15047,#2167);
#1799=LINE('',#15048,#2168);
#1800=LINE('',#15074,#2169);
#1801=LINE('',#15091,#2170);
#1802=LINE('',#15094,#2171);
#1803=LINE('',#15097,#2172);
#1804=LINE('',#15105,#2173);
#1805=LINE('',#15111,#2174);
#1806=LINE('',#15120,#2175);
#1807=LINE('',#15126,#2176);
#1808=LINE('',#15135,#2177);
#1809=LINE('',#15141,#2178);
#1810=LINE('',#15150,#2179);
#1811=LINE('',#15156,#2180);
#1812=LINE('',#15164,#2181);
#1813=LINE('',#15166,#2182);
#1814=LINE('',#15168,#2183);
#1815=LINE('',#15169,#2184);
#1816=LINE('',#15175,#2185);
#1817=LINE('',#15178,#2186);
#1818=LINE('',#15180,#2187);
#1819=LINE('',#15181,#2188);
#1820=LINE('',#15192,#2189);
#1821=LINE('',#15198,#2190);
#1822=LINE('',#15207,#2191);
#1823=LINE('',#15213,#2192);
#1824=LINE('',#15222,#2193);
#1825=LINE('',#15228,#2194);
#1826=LINE('',#15237,#2195);
#1827=LINE('',#15243,#2196);
#1828=LINE('',#15251,#2197);
#1829=LINE('',#15253,#2198);
#1830=LINE('',#15255,#2199);
#1831=LINE('',#15256,#2200);
#1832=LINE('',#15260,#2201);
#1833=LINE('',#15262,#2202);
#1834=LINE('',#15264,#2203);
#1835=LINE('',#15265,#2204);
#1836=LINE('',#15278,#2205);
#1837=LINE('',#15293,#2206);
#1838=LINE('',#15307,#2207);
#1839=LINE('',#15355,#2208);
#1840=LINE('',#15403,#2209);
#1841=LINE('',#15451,#2210);
#1842=LINE('',#15505,#2211);
#1843=LINE('',#15553,#2212);
#1844=LINE('',#15601,#2213);
#1845=LINE('',#15626,#2214);
#1846=LINE('',#15651,#2215);
#1847=LINE('',#15675,#2216);
#1848=LINE('',#15700,#2217);
#1849=LINE('',#15725,#2218);
#1850=LINE('',#15749,#2219);
#1851=LINE('',#15974,#2220);
#1852=LINE('',#16572,#2221);
#1853=LINE('',#16574,#2222);
#1854=LINE('',#16576,#2223);
#1855=LINE('',#16577,#2224);
#1856=LINE('',#16580,#2225);
#1857=LINE('',#16582,#2226);
#1858=LINE('',#16583,#2227);
#1859=LINE('',#16586,#2228);
#1860=LINE('',#16588,#2229);
#1861=LINE('',#16589,#2230);
#1862=LINE('',#16592,#2231);
#1863=LINE('',#16594,#2232);
#1864=LINE('',#16595,#2233);
#1865=LINE('',#16598,#2234);
#1866=LINE('',#16600,#2235);
#1867=LINE('',#16601,#2236);
#1868=LINE('',#16603,#2237);
#1869=LINE('',#16604,#2238);
#1870=LINE('',#16611,#2239);
#1871=VECTOR('',#6996,6.35);
#1872=VECTOR('',#7003,6.85);
#1873=VECTOR('',#7016,0.35);
#1874=VECTOR('',#7023,0.35);
#1875=VECTOR('',#7030,0.35);
#1876=VECTOR('',#7037,0.35);
#1877=VECTOR('',#7042,1.);
#1878=VECTOR('',#7043,1.);
#1879=VECTOR('',#7044,1.);
#1880=VECTOR('',#7045,1.);
#1881=VECTOR('',#7052,1.);
#1882=VECTOR('',#7055,1.);
#1883=VECTOR('',#7056,1.);
#1884=VECTOR('',#7057,1.);
#1885=VECTOR('',#7068,1.);
#1886=VECTOR('',#7069,1.);
#1887=VECTOR('',#7070,1.);
#1888=VECTOR('',#7071,1.);
#1889=VECTOR('',#7078,1.);
#1890=VECTOR('',#7081,1.);
#1891=VECTOR('',#7082,1.);
#1892=VECTOR('',#7083,1.);
#1893=VECTOR('',#7094,1.);
#1894=VECTOR('',#7095,1.);
#1895=VECTOR('',#7096,1.);
#1896=VECTOR('',#7097,1.);
#1897=VECTOR('',#7104,1.);
#1898=VECTOR('',#7107,1.);
#1899=VECTOR('',#7108,1.);
#1900=VECTOR('',#7109,1.);
#1901=VECTOR('',#7120,1.);
#1902=VECTOR('',#7121,1.);
#1903=VECTOR('',#7122,1.);
#1904=VECTOR('',#7123,1.);
#1905=VECTOR('',#7130,1.);
#1906=VECTOR('',#7133,1.);
#1907=VECTOR('',#7134,1.);
#1908=VECTOR('',#7135,1.);
#1909=VECTOR('',#7146,1.);
#1910=VECTOR('',#7147,1.);
#1911=VECTOR('',#7148,1.);
#1912=VECTOR('',#7149,1.);
#1913=VECTOR('',#7156,1.);
#1914=VECTOR('',#7159,1.);
#1915=VECTOR('',#7160,1.);
#1916=VECTOR('',#7161,1.);
#1917=VECTOR('',#7172,1.);
#1918=VECTOR('',#7173,1.);
#1919=VECTOR('',#7174,1.);
#1920=VECTOR('',#7175,1.);
#1921=VECTOR('',#7182,1.);
#1922=VECTOR('',#7185,1.);
#1923=VECTOR('',#7186,1.);
#1924=VECTOR('',#7187,1.);
#1925=VECTOR('',#7198,1.);
#1926=VECTOR('',#7199,1.);
#1927=VECTOR('',#7200,1.);
#1928=VECTOR('',#7201,1.);
#1929=VECTOR('',#7204,1.);
#1930=VECTOR('',#7205,1.);
#1931=VECTOR('',#7206,1.);
#1932=VECTOR('',#7207,1.);
#1933=VECTOR('',#7210,1.);
#1934=VECTOR('',#7211,1.);
#1935=VECTOR('',#7212,1.);
#1936=VECTOR('',#7213,1.);
#1937=VECTOR('',#7216,1.);
#1938=VECTOR('',#7217,1.);
#1939=VECTOR('',#7218,1.);
#1940=VECTOR('',#7219,1.);
#1941=VECTOR('',#7228,1.);
#1942=VECTOR('',#7231,1.);
#1943=VECTOR('',#7242,1.);
#1944=VECTOR('',#7249,1.);
#1945=VECTOR('',#7256,1.7);
#1946=VECTOR('',#7259,1.);
#1947=VECTOR('',#7262,1.);
#1948=VECTOR('',#7269,1.);
#1949=VECTOR('',#7272,1.);
#1950=VECTOR('',#7275,6.2);
#1951=VECTOR('',#7282,8.2);
#1952=VECTOR('',#7295,6.35);
#1953=VECTOR('',#7302,6.85);
#1954=VECTOR('',#7315,0.35);
#1955=VECTOR('',#7322,0.35);
#1956=VECTOR('',#7329,0.35);
#1957=VECTOR('',#7336,0.35);
#1958=VECTOR('',#7341,2.7);
#1959=VECTOR('',#7348,8.2);
#1960=VECTOR('',#7359,1.);
#1961=VECTOR('',#7360,1.);
#1962=VECTOR('',#7361,1.);
#1963=VECTOR('',#7362,1.);
#1964=VECTOR('',#7365,1.);
#1965=VECTOR('',#7366,1.);
#1966=VECTOR('',#7367,1.);
#1967=VECTOR('',#7370,1.);
#1968=VECTOR('',#7371,1.);
#1969=VECTOR('',#7372,1.);
#1970=VECTOR('',#7383,1.);
#1971=VECTOR('',#7386,1.);
#1972=VECTOR('',#7389,1.);
#1973=VECTOR('',#7392,1.);
#1974=VECTOR('',#7395,1.);
#1975=VECTOR('',#7398,1.);
#1976=VECTOR('',#7401,1.);
#1977=VECTOR('',#7404,1.);
#1978=VECTOR('',#7407,1.);
#1979=VECTOR('',#7410,1.);
#1980=VECTOR('',#7413,1.);
#1981=VECTOR('',#7416,1.);
#1982=VECTOR('',#7425,1.);
#1983=VECTOR('',#7426,1.);
#1984=VECTOR('',#7429,1.);
#1985=VECTOR('',#7430,1.);
#1986=VECTOR('',#7435,1.);
#1987=VECTOR('',#7438,1.);
#1988=VECTOR('',#7445,1.);
#1989=VECTOR('',#7446,1.);
#1990=VECTOR('',#7449,1.);
#1991=VECTOR('',#7450,1.);
#1992=VECTOR('',#7455,1.);
#1993=VECTOR('',#7458,1.);
#1994=VECTOR('',#7465,1.);
#1995=VECTOR('',#7466,1.);
#1996=VECTOR('',#7469,1.);
#1997=VECTOR('',#7470,1.);
#1998=VECTOR('',#7475,1.);
#1999=VECTOR('',#7478,1.);
#2000=VECTOR('',#7485,1.);
#2001=VECTOR('',#7486,1.);
#2002=VECTOR('',#7489,1.);
#2003=VECTOR('',#7490,1.);
#2004=VECTOR('',#7495,1.);
#2005=VECTOR('',#7498,1.);
#2006=VECTOR('',#7505,1.);
#2007=VECTOR('',#7506,1.);
#2008=VECTOR('',#7509,1.);
#2009=VECTOR('',#7510,1.);
#2010=VECTOR('',#7515,1.);
#2011=VECTOR('',#7518,1.);
#2012=VECTOR('',#7525,1.);
#2013=VECTOR('',#7526,1.);
#2014=VECTOR('',#7529,1.);
#2015=VECTOR('',#7530,1.);
#2016=VECTOR('',#7535,1.);
#2017=VECTOR('',#7538,1.);
#2018=VECTOR('',#7545,1.5);
#2019=VECTOR('',#7554,1.);
#2020=VECTOR('',#7559,5.);
#2021=VECTOR('',#7568,1.5);
#2022=VECTOR('',#7575,1.7);
#2023=VECTOR('',#7586,0.3);
#2024=VECTOR('',#7591,0.3);
#2025=VECTOR('',#7594,0.3);
#2026=VECTOR('',#7597,0.3);
#2027=VECTOR('',#7600,0.3);
#2028=VECTOR('',#7603,0.3);
#2029=VECTOR('',#7606,0.3);
#2030=VECTOR('',#7609,0.3);
#2031=VECTOR('',#7614,0.3);
#2032=VECTOR('',#7619,0.3);
#2033=VECTOR('',#7622,0.3);
#2034=VECTOR('',#7625,0.3);
#2035=VECTOR('',#7628,0.3);
#2036=VECTOR('',#7631,0.3);
#2037=VECTOR('',#7634,0.3);
#2038=VECTOR('',#7637,0.3);
#2039=VECTOR('',#7642,0.3);
#2040=VECTOR('',#7647,0.3);
#2041=VECTOR('',#7650,0.3);
#2042=VECTOR('',#7653,0.3);
#2043=VECTOR('',#7656,0.3);
#2044=VECTOR('',#7659,0.3);
#2045=VECTOR('',#7662,0.3);
#2046=VECTOR('',#7665,0.3);
#2047=VECTOR('',#7670,0.3);
#2048=VECTOR('',#7675,0.3);
#2049=VECTOR('',#7678,0.3);
#2050=VECTOR('',#7681,0.3);
#2051=VECTOR('',#7684,0.3);
#2052=VECTOR('',#7687,0.3);
#2053=VECTOR('',#7690,0.3);
#2054=VECTOR('',#7693,0.3);
#2055=VECTOR('',#7698,0.30735);
#2056=VECTOR('',#7703,0.30735);
#2057=VECTOR('',#7706,0.30735);
#2058=VECTOR('',#7709,0.30735);
#2059=VECTOR('',#7712,0.30735);
#2060=VECTOR('',#7715,0.30735);
#2061=VECTOR('',#7718,0.30735);
#2062=VECTOR('',#7721,0.30735);
#2063=VECTOR('',#7726,0.30735);
#2064=VECTOR('',#7731,0.30735);
#2065=VECTOR('',#7734,0.30735);
#2066=VECTOR('',#7737,0.30735);
#2067=VECTOR('',#7740,0.30735);
#2068=VECTOR('',#7743,0.30735);
#2069=VECTOR('',#7746,0.30735);
#2070=VECTOR('',#7749,0.30735);
#2071=VECTOR('',#7754,0.30735);
#2072=VECTOR('',#7759,0.30735);
#2073=VECTOR('',#7762,0.30735);
#2074=VECTOR('',#7765,0.30735);
#2075=VECTOR('',#7768,0.30735);
#2076=VECTOR('',#7771,0.30735);
#2077=VECTOR('',#7774,0.30735);
#2078=VECTOR('',#7777,0.30735);
#2079=VECTOR('',#7782,0.30735);
#2080=VECTOR('',#7787,0.30735);
#2081=VECTOR('',#7790,0.30735);
#2082=VECTOR('',#7793,0.30735);
#2083=VECTOR('',#7796,0.30735);
#2084=VECTOR('',#7799,0.30735);
#2085=VECTOR('',#7802,0.30735);
#2086=VECTOR('',#7805,0.30735);
#2087=VECTOR('',#7812,6.35);
#2088=VECTOR('',#7819,6.85);
#2089=VECTOR('',#7830,1.);
#2090=VECTOR('',#7833,1.);
#2091=VECTOR('',#7836,1.);
#2092=VECTOR('',#7839,1.);
#2093=VECTOR('',#7840,1.);
#2094=VECTOR('',#7843,1.);
#2095=VECTOR('',#7874,0.35);
#2096=VECTOR('',#7881,0.35);
#2097=VECTOR('',#7888,0.35);
#2098=VECTOR('',#7895,0.35);
#2099=VECTOR('',#7906,4.8);
#2100=VECTOR('',#7915,3.5);
#2101=VECTOR('',#7918,1.);
#2102=VECTOR('',#7919,1.);
#2103=VECTOR('',#7920,1.);
#2104=VECTOR('',#7923,1.);
#2105=VECTOR('',#7924,1.);
#2106=VECTOR('',#7925,1.);
#2107=VECTOR('',#7928,1.);
#2108=VECTOR('',#7929,1.);
#2109=VECTOR('',#7930,1.);
#2110=VECTOR('',#7933,1.);
#2111=VECTOR('',#7934,1.);
#2112=VECTOR('',#7935,1.);
#2113=VECTOR('',#7938,1.);
#2114=VECTOR('',#7941,1.);
#2115=VECTOR('',#7944,2.7);
#2116=VECTOR('',#7949,1.);
#2117=VECTOR('',#7956,1.);
#2118=VECTOR('',#7961,1.);
#2119=VECTOR('',#7966,1.7);
#2120=VECTOR('',#7969,1.);
#2121=VECTOR('',#7980,8.2);
#2122=VECTOR('',#8005,0.35);
#2123=VECTOR('',#8010,0.35);
#2124=VECTOR('',#8015,0.35);
#2125=VECTOR('',#8020,0.35);
#2126=VECTOR('',#8031,3.);
#2127=VECTOR('',#8034,1.);
#2128=VECTOR('',#8041,1.);
#2129=VECTOR('',#8044,1.8);
#2130=VECTOR('',#8047,1.);
#2131=VECTOR('',#8048,1.);
#2132=VECTOR('',#8053,6.2);
#2133=VECTOR('',#8062,8.2);
#2134=VECTOR('',#8069,0.35);
#2135=VECTOR('',#8076,0.35);
#2136=VECTOR('',#8083,0.35);
#2137=VECTOR('',#8090,0.35);
#2138=VECTOR('',#8097,1.7);
#2139=VECTOR('',#8112,1.1);
#2140=VECTOR('',#8119,2.1);
#2141=VECTOR('',#8128,1.7);
#2142=VECTOR('',#8137,1.);
#2143=VECTOR('',#8140,1.);
#2144=VECTOR('',#8143,1.);
#2145=VECTOR('',#8146,1.);
#2146=VECTOR('',#8149,1.);
#2147=VECTOR('',#8150,1.);
#2148=VECTOR('',#8151,1.);
#2149=VECTOR('',#8156,1.);
#2150=VECTOR('',#8159,1.);
#2151=VECTOR('',#8160,1.);
#2152=VECTOR('',#8169,1.);
#2153=VECTOR('',#8174,1.);
#2154=VECTOR('',#8175,1.);
#2155=VECTOR('',#8176,1.);
#2156=VECTOR('',#8177,1.);
#2157=VECTOR('',#8182,1.);
#2158=VECTOR('',#8185,1.);
#2159=VECTOR('',#8186,1.);
#2160=VECTOR('',#8187,1.);
#2161=VECTOR('',#8196,1.);
#2162=VECTOR('',#8197,1.);
#2163=VECTOR('',#8198,1.);
#2164=VECTOR('',#8199,1.);
#2165=VECTOR('',#8204,1.);
#2166=VECTOR('',#8207,1.);
#2167=VECTOR('',#8208,1.);
#2168=VECTOR('',#8209,1.);
#2169=VECTOR('',#8220,0.9);
#2170=VECTOR('',#8243,1.4);
#2171=VECTOR('',#8246,1.);
#2172=VECTOR('',#8251,1.);
#2173=VECTOR('',#8262,1.);
#2174=VECTOR('',#8269,1.5);
#2175=VECTOR('',#8282,1.);
#2176=VECTOR('',#8289,1.5);
#2177=VECTOR('',#8302,1.);
#2178=VECTOR('',#8309,1.5);
#2179=VECTOR('',#8322,1.);
#2180=VECTOR('',#8329,1.7);
#2181=VECTOR('',#8340,1.);
#2182=VECTOR('',#8341,1.);
#2183=VECTOR('',#8342,1.);
#2184=VECTOR('',#8343,1.);
#2185=VECTOR('',#8350,1.);
#2186=VECTOR('',#8353,1.);
#2187=VECTOR('',#8354,1.);
#2188=VECTOR('',#8355,1.);
#2189=VECTOR('',#8372,1.);
#2190=VECTOR('',#8379,1.7);
#2191=VECTOR('',#8392,1.);
#2192=VECTOR('',#8399,1.5);
#2193=VECTOR('',#8412,1.1);
#2194=VECTOR('',#8419,1.7);
#2195=VECTOR('',#8432,1.);
#2196=VECTOR('',#8439,1.4);
#2197=VECTOR('',#8450,1.);
#2198=VECTOR('',#8451,1.);
#2199=VECTOR('',#8452,1.);
#2200=VECTOR('',#8453,1.);
#2201=VECTOR('',#8456,1.);
#2202=VECTOR('',#8457,1.);
#2203=VECTOR('',#8458,1.);
#2204=VECTOR('',#8459,1.);
#2205=VECTOR('',#8480,0.3);
#2206=VECTOR('',#8483,0.3);
#2207=VECTOR('',#8490,0.3);
#2208=VECTOR('',#8493,0.3);
#2209=VECTOR('',#8496,0.3);
#2210=VECTOR('',#8499,0.3);
#2211=VECTOR('',#8502,0.3);
#2212=VECTOR('',#8505,0.3);
#2213=VECTOR('',#8508,0.237175);
#2214=VECTOR('',#8513,0.237175);
#2215=VECTOR('',#8516,0.237175);
#2216=VECTOR('',#8519,0.237175);
#2217=VECTOR('',#8522,0.237175);
#2218=VECTOR('',#8525,0.237175);
#2219=VECTOR('',#8528,0.237175);
#2220=VECTOR('',#8533,0.25);
#2221=VECTOR('',#8546,1.);
#2222=VECTOR('',#8547,1.);
#2223=VECTOR('',#8548,1.);
#2224=VECTOR('',#8549,1.);
#2225=VECTOR('',#8552,1.);
#2226=VECTOR('',#8553,1.);
#2227=VECTOR('',#8554,1.);
#2228=VECTOR('',#8557,1.);
#2229=VECTOR('',#8558,1.);
#2230=VECTOR('',#8559,1.);
#2231=VECTOR('',#8562,1.);
#2232=VECTOR('',#8563,1.);
#2233=VECTOR('',#8564,1.);
#2234=VECTOR('',#8567,1.);
#2235=VECTOR('',#8568,1.);
#2236=VECTOR('',#8569,1.);
#2237=VECTOR('',#8572,1.);
#2238=VECTOR('',#8573,1.);
#2239=VECTOR('',#8582,0.5);
#2240=CIRCLE('',#6344,6.35);
#2241=CIRCLE('',#6345,6.35);
#2242=CIRCLE('',#6347,6.85);
#2243=CIRCLE('',#6348,6.85);
#2244=CIRCLE('',#6351,6.2);
#2245=CIRCLE('',#6353,0.35);
#2246=CIRCLE('',#6354,0.35);
#2247=CIRCLE('',#6356,0.35);
#2248=CIRCLE('',#6357,0.35);
#2249=CIRCLE('',#6359,0.35);
#2250=CIRCLE('',#6360,0.35);
#2251=CIRCLE('',#6362,0.35);
#2252=CIRCLE('',#6363,0.35);
#2253=CIRCLE('',#6366,2.9);
#2254=CIRCLE('',#6367,2.9);
#2255=CIRCLE('',#6370,3.2);
#2256=CIRCLE('',#6371,3.2);
#2257=CIRCLE('',#6375,2.9);
#2258=CIRCLE('',#6376,2.9);
#2259=CIRCLE('',#6379,3.2);
#2260=CIRCLE('',#6380,3.2);
#2261=CIRCLE('',#6384,2.9);
#2262=CIRCLE('',#6385,2.9);
#2263=CIRCLE('',#6388,3.2);
#2264=CIRCLE('',#6389,3.2);
#2265=CIRCLE('',#6393,2.9);
#2266=CIRCLE('',#6394,2.9);
#2267=CIRCLE('',#6397,3.2);
#2268=CIRCLE('',#6398,3.2);
#2269=CIRCLE('',#6402,2.9);
#2270=CIRCLE('',#6403,2.9);
#2271=CIRCLE('',#6406,3.2);
#2272=CIRCLE('',#6407,3.2);
#2273=CIRCLE('',#6411,2.9);
#2274=CIRCLE('',#6412,2.9);
#2275=CIRCLE('',#6415,3.2);
#2276=CIRCLE('',#6416,3.2);
#2277=CIRCLE('',#6423,5.8);
#2278=CIRCLE('',#6424,6.2);
#2279=CIRCLE('',#6425,5.8);
#2280=CIRCLE('',#6426,6.2);
#2281=CIRCLE('',#6427,5.8);
#2282=CIRCLE('',#6428,6.2);
#2283=CIRCLE('',#6429,1.7);
#2284=CIRCLE('',#6431,5.8);
#2285=CIRCLE('',#6433,5.8);
#2286=CIRCLE('',#6435,5.8);
#2287=CIRCLE('',#6437,1.7);
#2288=CIRCLE('',#6439,6.2);
#2289=CIRCLE('',#6440,6.2);
#2290=CIRCLE('',#6441,6.2);
#2291=CIRCLE('',#6445,6.2);
#2292=CIRCLE('',#6447,8.2);
#2293=CIRCLE('',#6448,8.2);
#2294=CIRCLE('',#6453,6.35);
#2295=CIRCLE('',#6454,6.35);
#2296=CIRCLE('',#6456,6.85);
#2297=CIRCLE('',#6457,6.85);
#2298=CIRCLE('',#6460,2.7);
#2299=CIRCLE('',#6462,0.35);
#2300=CIRCLE('',#6463,0.35);
#2301=CIRCLE('',#6465,0.35);
#2302=CIRCLE('',#6466,0.35);
#2303=CIRCLE('',#6468,0.35);
#2304=CIRCLE('',#6469,0.35);
#2305=CIRCLE('',#6471,0.35);
#2306=CIRCLE('',#6472,0.35);
#2307=CIRCLE('',#6474,2.7);
#2308=CIRCLE('',#6476,8.2);
#2309=CIRCLE('',#6477,8.2);
#2310=CIRCLE('',#6485,1.);
#2311=CIRCLE('',#6487,5.);
#2312=CIRCLE('',#6488,2.9);
#2313=CIRCLE('',#6489,3.2);
#2314=CIRCLE('',#6490,2.9);
#2315=CIRCLE('',#6491,3.2);
#2316=CIRCLE('',#6492,2.9);
#2317=CIRCLE('',#6493,3.2);
#2318=CIRCLE('',#6494,2.9);
#2319=CIRCLE('',#6495,3.2);
#2320=CIRCLE('',#6496,2.9);
#2321=CIRCLE('',#6497,3.2);
#2322=CIRCLE('',#6498,2.9);
#2323=CIRCLE('',#6499,3.2);
#2324=CIRCLE('',#6500,1.);
#2325=CIRCLE('',#6501,1.);
#2326=CIRCLE('',#6503,2.9);
#2327=CIRCLE('',#6506,3.2);
#2328=CIRCLE('',#6510,2.9);
#2329=CIRCLE('',#6513,3.2);
#2330=CIRCLE('',#6517,2.9);
#2331=CIRCLE('',#6520,3.2);
#2332=CIRCLE('',#6524,2.9);
#2333=CIRCLE('',#6527,3.2);
#2334=CIRCLE('',#6531,2.9);
#2335=CIRCLE('',#6534,3.2);
#2336=CIRCLE('',#6538,2.9);
#2337=CIRCLE('',#6541,3.2);
#2338=CIRCLE('',#6545,1.5);
#2339=CIRCLE('',#6546,1.5);
#2340=CIRCLE('',#6548,1.);
#2341=CIRCLE('',#6551,5.);
#2342=CIRCLE('',#6555,1.5);
#2343=CIRCLE('',#6556,1.5);
#2344=CIRCLE('',#6558,1.7);
#2345=CIRCLE('',#6559,1.7);
#2346=CIRCLE('',#6564,0.25175);
#2347=CIRCLE('',#6572,0.25175);
#2348=CIRCLE('',#6574,0.25175);
#2349=CIRCLE('',#6582,0.25175);
#2350=CIRCLE('',#6584,0.25175);
#2351=CIRCLE('',#6592,0.25175);
#2352=CIRCLE('',#6594,0.25175);
#2353=CIRCLE('',#6602,0.25175);
#2354=CIRCLE('',#6604,0.30735);
#2355=CIRCLE('',#6612,0.30735);
#2356=CIRCLE('',#6614,0.30735);
#2357=CIRCLE('',#6622,0.30735);
#2358=CIRCLE('',#6624,0.30735);
#2359=CIRCLE('',#6632,0.30735);
#2360=CIRCLE('',#6634,0.30735);
#2361=CIRCLE('',#6642,0.30735);
#2362=CIRCLE('',#6644,6.35);
#2363=CIRCLE('',#6645,6.35);
#2364=CIRCLE('',#6647,6.85);
#2365=CIRCLE('',#6648,6.85);
#2366=CIRCLE('',#6651,2.7);
#2367=CIRCLE('',#6652,2.7);
#2368=CIRCLE('',#6653,2.1);
#2369=CIRCLE('',#6654,2.7);
#2370=CIRCLE('',#6655,2.1);
#2371=CIRCLE('',#6656,2.1);
#2372=CIRCLE('',#6657,2.7);
#2373=CIRCLE('',#6658,1.7);
#2374=CIRCLE('',#6661,8.2);
#2375=CIRCLE('',#6662,3.5);
#2376=CIRCLE('',#6671,0.35);
#2377=CIRCLE('',#6672,0.35);
#2378=CIRCLE('',#6674,0.35);
#2379=CIRCLE('',#6675,0.35);
#2380=CIRCLE('',#6677,0.35);
#2381=CIRCLE('',#6678,0.35);
#2382=CIRCLE('',#6680,0.35);
#2383=CIRCLE('',#6681,0.35);
#2384=CIRCLE('',#6683,4.8);
#2385=CIRCLE('',#6684,3.5);
#2386=CIRCLE('',#6686,4.8);
#2387=CIRCLE('',#6688,2.7);
#2388=CIRCLE('',#6695,2.7);
#2389=CIRCLE('',#6696,2.7);
#2390=CIRCLE('',#6697,2.7);
#2391=CIRCLE('',#6699,2.1);
#2392=CIRCLE('',#6700,2.1);
#2393=CIRCLE('',#6701,2.1);
#2394=CIRCLE('',#6702,1.7);
#2395=CIRCLE('',#6709,8.2);
#2396=CIRCLE('',#6714,6.375);
#2397=CIRCLE('',#6717,3.);
#2398=CIRCLE('',#6718,0.35);
#2399=CIRCLE('',#6719,0.35);
#2400=CIRCLE('',#6720,0.35);
#2401=CIRCLE('',#6721,1.);
#2402=CIRCLE('',#6722,0.35);
#2403=CIRCLE('',#6724,0.35);
#2404=CIRCLE('',#6726,0.35);
#2405=CIRCLE('',#6728,0.35);
#2406=CIRCLE('',#6730,0.35);
#2407=CIRCLE('',#6732,3.);
#2408=CIRCLE('',#6733,1.8);
#2409=CIRCLE('',#6736,1.8);
#2410=CIRCLE('',#6737,1.);
#2411=CIRCLE('',#6742,6.2);
#2412=CIRCLE('',#6743,6.2);
#2413=CIRCLE('',#6744,6.2);
#2414=CIRCLE('',#6746,8.2);
#2415=CIRCLE('',#6747,8.2);
#2416=CIRCLE('',#6749,0.35);
#2417=CIRCLE('',#6750,0.35);
#2418=CIRCLE('',#6752,0.35);
#2419=CIRCLE('',#6753,0.35);
#2420=CIRCLE('',#6755,0.35);
#2421=CIRCLE('',#6756,0.35);
#2422=CIRCLE('',#6758,0.35);
#2423=CIRCLE('',#6759,0.35);
#2424=CIRCLE('',#6761,1.7);
#2425=CIRCLE('',#6762,1.7);
#2426=CIRCLE('',#6764,2.1);
#2427=CIRCLE('',#6766,1.7);
#2428=CIRCLE('',#6767,1.1);
#2429=CIRCLE('',#6769,1.1);
#2430=CIRCLE('',#6771,2.1);
#2431=CIRCLE('',#6775,1.7);
#2432=CIRCLE('',#6780,0.3);
#2433=CIRCLE('',#6782,0.3);
#2434=CIRCLE('',#6785,0.3);
#2435=CIRCLE('',#6789,1.);
#2436=CIRCLE('',#6790,1.);
#2437=CIRCLE('',#6791,1.);
#2438=CIRCLE('',#6794,0.3);
#2439=CIRCLE('',#6797,0.3);
#2440=CIRCLE('',#6801,0.3);
#2441=CIRCLE('',#6804,0.3);
#2442=CIRCLE('',#6807,0.9);
#2443=CIRCLE('',#6808,0.9);
#2444=CIRCLE('',#6810,1.);
#2445=CIRCLE('',#6813,1.4);
#2446=CIRCLE('',#6814,1.);
#2447=CIRCLE('',#6816,1.4);
#2448=CIRCLE('',#6817,1.);
#2449=CIRCLE('',#6820,1.);
#2450=CIRCLE('',#6826,1.);
#2451=CIRCLE('',#6827,1.);
#2452=CIRCLE('',#6829,1.5);
#2453=CIRCLE('',#6830,1.5);
#2454=CIRCLE('',#6835,1.);
#2455=CIRCLE('',#6836,1.);
#2456=CIRCLE('',#6838,1.5);
#2457=CIRCLE('',#6839,1.5);
#2458=CIRCLE('',#6844,1.);
#2459=CIRCLE('',#6845,1.);
#2460=CIRCLE('',#6847,1.5);
#2461=CIRCLE('',#6848,1.5);
#2462=CIRCLE('',#6853,1.);
#2463=CIRCLE('',#6854,1.);
#2464=CIRCLE('',#6856,1.7);
#2465=CIRCLE('',#6857,1.7);
#2466=CIRCLE('',#6863,0.3);
#2467=CIRCLE('',#6864,0.3);
#2468=CIRCLE('',#6867,0.3);
#2469=CIRCLE('',#6868,0.3);
#2470=CIRCLE('',#6873,1.);
#2471=CIRCLE('',#6874,1.);
#2472=CIRCLE('',#6876,1.7);
#2473=CIRCLE('',#6877,1.7);
#2474=CIRCLE('',#6882,1.);
#2475=CIRCLE('',#6883,1.);
#2476=CIRCLE('',#6885,1.5);
#2477=CIRCLE('',#6886,1.5);
#2478=CIRCLE('',#6891,1.1);
#2479=CIRCLE('',#6892,1.1);
#2480=CIRCLE('',#6894,1.7);
#2481=CIRCLE('',#6895,1.7);
#2482=CIRCLE('',#6900,1.);
#2483=CIRCLE('',#6901,1.);
#2484=CIRCLE('',#6903,1.4);
#2485=CIRCLE('',#6904,1.4);
#2486=CIRCLE('',#6911,1.4);
#2487=CIRCLE('',#6912,0.9);
#2488=CIRCLE('',#6914,0.9);
#2489=CIRCLE('',#6916,1.4);
#2490=CIRCLE('',#6920,0.2942);
#2491=CIRCLE('',#6921,0.2942);
#2492=CIRCLE('',#6922,0.2942);
#2493=CIRCLE('',#6930,0.237175);
#2494=CIRCLE('',#6938,0.2942);
#2495=CIRCLE('',#6939,0.199999999999999);
#2496=CIRCLE('',#6941,0.237175);
#2497=CIRCLE('',#6952,0.5);
#2498=CIRCLE('',#6954,0.5);
#2499=VERTEX_POINT('',#8654);
#2500=VERTEX_POINT('',#8656);
#2501=VERTEX_POINT('',#8660);
#2502=VERTEX_POINT('',#8662);
#2503=VERTEX_POINT('',#8667);
#2504=VERTEX_POINT('',#8670);
#2505=VERTEX_POINT('',#8672);
#2506=VERTEX_POINT('',#8676);
#2507=VERTEX_POINT('',#8678);
#2508=VERTEX_POINT('',#8682);
#2509=VERTEX_POINT('',#8684);
#2510=VERTEX_POINT('',#8688);
#2511=VERTEX_POINT('',#8690);
#2512=VERTEX_POINT('',#8694);
#2513=VERTEX_POINT('',#8695);
#2514=VERTEX_POINT('',#8697);
#2515=VERTEX_POINT('',#8699);
#2516=VERTEX_POINT('',#8703);
#2517=VERTEX_POINT('',#8705);
#2518=VERTEX_POINT('',#8709);
#2519=VERTEX_POINT('',#8711);
#2520=VERTEX_POINT('',#8719);
#2521=VERTEX_POINT('',#8720);
#2522=VERTEX_POINT('',#8722);
#2523=VERTEX_POINT('',#8724);
#2524=VERTEX_POINT('',#8728);
#2525=VERTEX_POINT('',#8730);
#2526=VERTEX_POINT('',#8734);
#2527=VERTEX_POINT('',#8736);
#2528=VERTEX_POINT('',#8744);
#2529=VERTEX_POINT('',#8745);
#2530=VERTEX_POINT('',#8747);
#2531=VERTEX_POINT('',#8749);
#2532=VERTEX_POINT('',#8753);
#2533=VERTEX_POINT('',#8755);
#2534=VERTEX_POINT('',#8759);
#2535=VERTEX_POINT('',#8761);
#2536=VERTEX_POINT('',#8769);
#2537=VERTEX_POINT('',#8770);
#2538=VERTEX_POINT('',#8772);
#2539=VERTEX_POINT('',#8774);
#2540=VERTEX_POINT('',#8778);
#2541=VERTEX_POINT('',#8780);
#2542=VERTEX_POINT('',#8784);
#2543=VERTEX_POINT('',#8786);
#2544=VERTEX_POINT('',#8794);
#2545=VERTEX_POINT('',#8795);
#2546=VERTEX_POINT('',#8797);
#2547=VERTEX_POINT('',#8799);
#2548=VERTEX_POINT('',#8803);
#2549=VERTEX_POINT('',#8805);
#2550=VERTEX_POINT('',#8809);
#2551=VERTEX_POINT('',#8811);
#2552=VERTEX_POINT('',#8819);
#2553=VERTEX_POINT('',#8820);
#2554=VERTEX_POINT('',#8822);
#2555=VERTEX_POINT('',#8824);
#2556=VERTEX_POINT('',#8828);
#2557=VERTEX_POINT('',#8830);
#2558=VERTEX_POINT('',#8834);
#2559=VERTEX_POINT('',#8836);
#2560=VERTEX_POINT('',#8844);
#2561=VERTEX_POINT('',#8845);
#2562=VERTEX_POINT('',#8847);
#2563=VERTEX_POINT('',#8849);
#2564=VERTEX_POINT('',#8853);
#2565=VERTEX_POINT('',#8854);
#2566=VERTEX_POINT('',#8856);
#2567=VERTEX_POINT('',#8858);
#2568=VERTEX_POINT('',#8862);
#2569=VERTEX_POINT('',#8863);
#2570=VERTEX_POINT('',#8865);
#2571=VERTEX_POINT('',#8867);
#2572=VERTEX_POINT('',#8871);
#2573=VERTEX_POINT('',#8872);
#2574=VERTEX_POINT('',#8874);
#2575=VERTEX_POINT('',#8876);
#2576=VERTEX_POINT('',#8882);
#2577=VERTEX_POINT('',#8884);
#2578=VERTEX_POINT('',#8886);
#2579=VERTEX_POINT('',#8888);
#2580=VERTEX_POINT('',#8892);
#2581=VERTEX_POINT('',#8895);
#2582=VERTEX_POINT('',#8901);
#2583=VERTEX_POINT('',#8905);
#2584=VERTEX_POINT('',#8909);
#2585=VERTEX_POINT('',#8911);
#2586=VERTEX_POINT('',#8921);
#2587=VERTEX_POINT('',#8925);
#2588=VERTEX_POINT('',#8927);
#2589=VERTEX_POINT('',#8934);
#2590=VERTEX_POINT('',#8936);
#2591=VERTEX_POINT('',#8940);
#2592=VERTEX_POINT('',#8942);
#2593=VERTEX_POINT('',#8947);
#2594=VERTEX_POINT('',#8950);
#2595=VERTEX_POINT('',#8952);
#2596=VERTEX_POINT('',#8956);
#2597=VERTEX_POINT('',#8958);
#2598=VERTEX_POINT('',#8962);
#2599=VERTEX_POINT('',#8964);
#2600=VERTEX_POINT('',#8968);
#2601=VERTEX_POINT('',#8970);
#2602=VERTEX_POINT('',#8974);
#2603=VERTEX_POINT('',#8978);
#2604=VERTEX_POINT('',#8980);
#2605=VERTEX_POINT('',#8987);
#2606=VERTEX_POINT('',#8988);
#2607=VERTEX_POINT('',#8990);
#2608=VERTEX_POINT('',#8992);
#2609=VERTEX_POINT('',#8996);
#2610=VERTEX_POINT('',#8998);
#2611=VERTEX_POINT('',#9002);
#2612=VERTEX_POINT('',#9003);
#2613=VERTEX_POINT('',#9010);
#2614=VERTEX_POINT('',#9012);
#2615=VERTEX_POINT('',#9013);
#2616=VERTEX_POINT('',#9015);
#2617=VERTEX_POINT('',#9017);
#2618=VERTEX_POINT('',#9020);
#2619=VERTEX_POINT('',#9021);
#2620=VERTEX_POINT('',#9023);
#2621=VERTEX_POINT('',#9025);
#2622=VERTEX_POINT('',#9028);
#2623=VERTEX_POINT('',#9029);
#2624=VERTEX_POINT('',#9031);
#2625=VERTEX_POINT('',#9033);
#2626=VERTEX_POINT('',#9036);
#2627=VERTEX_POINT('',#9037);
#2628=VERTEX_POINT('',#9039);
#2629=VERTEX_POINT('',#9041);
#2630=VERTEX_POINT('',#9044);
#2631=VERTEX_POINT('',#9045);
#2632=VERTEX_POINT('',#9047);
#2633=VERTEX_POINT('',#9049);
#2634=VERTEX_POINT('',#9052);
#2635=VERTEX_POINT('',#9053);
#2636=VERTEX_POINT('',#9055);
#2637=VERTEX_POINT('',#9057);
#2638=VERTEX_POINT('',#9060);
#2639=VERTEX_POINT('',#9064);
#2640=VERTEX_POINT('',#9065);
#2641=VERTEX_POINT('',#9070);
#2642=VERTEX_POINT('',#9074);
#2643=VERTEX_POINT('',#9081);
#2644=VERTEX_POINT('',#9082);
#2645=VERTEX_POINT('',#9087);
#2646=VERTEX_POINT('',#9091);
#2647=VERTEX_POINT('',#9098);
#2648=VERTEX_POINT('',#9099);
#2649=VERTEX_POINT('',#9104);
#2650=VERTEX_POINT('',#9108);
#2651=VERTEX_POINT('',#9115);
#2652=VERTEX_POINT('',#9116);
#2653=VERTEX_POINT('',#9121);
#2654=VERTEX_POINT('',#9125);
#2655=VERTEX_POINT('',#9132);
#2656=VERTEX_POINT('',#9133);
#2657=VERTEX_POINT('',#9138);
#2658=VERTEX_POINT('',#9142);
#2659=VERTEX_POINT('',#9149);
#2660=VERTEX_POINT('',#9150);
#2661=VERTEX_POINT('',#9155);
#2662=VERTEX_POINT('',#9159);
#2663=VERTEX_POINT('',#9166);
#2664=VERTEX_POINT('',#9168);
#2665=VERTEX_POINT('',#9172);
#2666=VERTEX_POINT('',#9177);
#2667=VERTEX_POINT('',#9183);
#2668=VERTEX_POINT('',#9185);
#2669=VERTEX_POINT('',#9189);
#2670=VERTEX_POINT('',#9191);
#2671=VERTEX_POINT('',#9198);
#2672=VERTEX_POINT('',#9199);
#2673=VERTEX_POINT('',#9201);
#2674=VERTEX_POINT('',#9206);
#2675=VERTEX_POINT('',#9219);
#2676=VERTEX_POINT('',#9220);
#2677=VERTEX_POINT('',#9270);
#2678=VERTEX_POINT('',#9271);
#2679=VERTEX_POINT('',#9321);
#2680=VERTEX_POINT('',#9322);
#2681=VERTEX_POINT('',#9369);
#2682=VERTEX_POINT('',#9370);
#2683=VERTEX_POINT('',#9420);
#2684=VERTEX_POINT('',#9421);
#2685=VERTEX_POINT('',#9471);
#2686=VERTEX_POINT('',#9472);
#2687=VERTEX_POINT('',#9519);
#2688=VERTEX_POINT('',#9520);
#2689=VERTEX_POINT('',#9522);
#2690=VERTEX_POINT('',#9536);
#2691=VERTEX_POINT('',#9558);
#2692=VERTEX_POINT('',#9559);
#2693=VERTEX_POINT('',#9561);
#2694=VERTEX_POINT('',#9566);
#2695=VERTEX_POINT('',#9579);
#2696=VERTEX_POINT('',#9580);
#2697=VERTEX_POINT('',#9630);
#2698=VERTEX_POINT('',#9631);
#2699=VERTEX_POINT('',#9681);
#2700=VERTEX_POINT('',#9682);
#2701=VERTEX_POINT('',#9729);
#2702=VERTEX_POINT('',#9730);
#2703=VERTEX_POINT('',#9780);
#2704=VERTEX_POINT('',#9781);
#2705=VERTEX_POINT('',#9831);
#2706=VERTEX_POINT('',#9832);
#2707=VERTEX_POINT('',#9879);
#2708=VERTEX_POINT('',#9880);
#2709=VERTEX_POINT('',#9882);
#2710=VERTEX_POINT('',#9896);
#2711=VERTEX_POINT('',#9918);
#2712=VERTEX_POINT('',#9919);
#2713=VERTEX_POINT('',#9921);
#2714=VERTEX_POINT('',#9926);
#2715=VERTEX_POINT('',#9939);
#2716=VERTEX_POINT('',#9940);
#2717=VERTEX_POINT('',#9990);
#2718=VERTEX_POINT('',#9991);
#2719=VERTEX_POINT('',#10041);
#2720=VERTEX_POINT('',#10042);
#2721=VERTEX_POINT('',#10089);
#2722=VERTEX_POINT('',#10090);
#2723=VERTEX_POINT('',#10140);
#2724=VERTEX_POINT('',#10141);
#2725=VERTEX_POINT('',#10191);
#2726=VERTEX_POINT('',#10192);
#2727=VERTEX_POINT('',#10239);
#2728=VERTEX_POINT('',#10240);
#2729=VERTEX_POINT('',#10242);
#2730=VERTEX_POINT('',#10256);
#2731=VERTEX_POINT('',#10278);
#2732=VERTEX_POINT('',#10279);
#2733=VERTEX_POINT('',#10281);
#2734=VERTEX_POINT('',#10286);
#2735=VERTEX_POINT('',#10299);
#2736=VERTEX_POINT('',#10300);
#2737=VERTEX_POINT('',#10350);
#2738=VERTEX_POINT('',#10351);
#2739=VERTEX_POINT('',#10401);
#2740=VERTEX_POINT('',#10402);
#2741=VERTEX_POINT('',#10449);
#2742=VERTEX_POINT('',#10450);
#2743=VERTEX_POINT('',#10500);
#2744=VERTEX_POINT('',#10501);
#2745=VERTEX_POINT('',#10551);
#2746=VERTEX_POINT('',#10552);
#2747=VERTEX_POINT('',#10599);
#2748=VERTEX_POINT('',#10600);
#2749=VERTEX_POINT('',#10602);
#2750=VERTEX_POINT('',#10616);
#2751=VERTEX_POINT('',#10638);
#2752=VERTEX_POINT('',#10639);
#2753=VERTEX_POINT('',#10641);
#2754=VERTEX_POINT('',#10650);
#2755=VERTEX_POINT('',#10662);
#2756=VERTEX_POINT('',#10663);
#2757=VERTEX_POINT('',#10686);
#2758=VERTEX_POINT('',#10687);
#2759=VERTEX_POINT('',#10711);
#2760=VERTEX_POINT('',#10712);
#2761=VERTEX_POINT('',#10736);
#2762=VERTEX_POINT('',#10737);
#2763=VERTEX_POINT('',#10760);
#2764=VERTEX_POINT('',#10761);
#2765=VERTEX_POINT('',#10785);
#2766=VERTEX_POINT('',#10786);
#2767=VERTEX_POINT('',#10810);
#2768=VERTEX_POINT('',#10811);
#2769=VERTEX_POINT('',#10813);
#2770=VERTEX_POINT('',#10819);
#2771=VERTEX_POINT('',#10827);
#2772=VERTEX_POINT('',#10828);
#2773=VERTEX_POINT('',#10830);
#2774=VERTEX_POINT('',#10839);
#2775=VERTEX_POINT('',#10851);
#2776=VERTEX_POINT('',#10852);
#2777=VERTEX_POINT('',#10875);
#2778=VERTEX_POINT('',#10876);
#2779=VERTEX_POINT('',#10900);
#2780=VERTEX_POINT('',#10901);
#2781=VERTEX_POINT('',#10925);
#2782=VERTEX_POINT('',#10926);
#2783=VERTEX_POINT('',#10949);
#2784=VERTEX_POINT('',#10950);
#2785=VERTEX_POINT('',#10974);
#2786=VERTEX_POINT('',#10975);
#2787=VERTEX_POINT('',#10999);
#2788=VERTEX_POINT('',#11000);
#2789=VERTEX_POINT('',#11002);
#2790=VERTEX_POINT('',#11008);
#2791=VERTEX_POINT('',#11016);
#2792=VERTEX_POINT('',#11017);
#2793=VERTEX_POINT('',#11019);
#2794=VERTEX_POINT('',#11028);
#2795=VERTEX_POINT('',#11040);
#2796=VERTEX_POINT('',#11041);
#2797=VERTEX_POINT('',#11064);
#2798=VERTEX_POINT('',#11065);
#2799=VERTEX_POINT('',#11089);
#2800=VERTEX_POINT('',#11090);
#2801=VERTEX_POINT('',#11114);
#2802=VERTEX_POINT('',#11115);
#2803=VERTEX_POINT('',#11138);
#2804=VERTEX_POINT('',#11139);
#2805=VERTEX_POINT('',#11163);
#2806=VERTEX_POINT('',#11164);
#2807=VERTEX_POINT('',#11188);
#2808=VERTEX_POINT('',#11189);
#2809=VERTEX_POINT('',#11191);
#2810=VERTEX_POINT('',#11197);
#2811=VERTEX_POINT('',#11205);
#2812=VERTEX_POINT('',#11206);
#2813=VERTEX_POINT('',#11208);
#2814=VERTEX_POINT('',#11217);
#2815=VERTEX_POINT('',#11229);
#2816=VERTEX_POINT('',#11230);
#2817=VERTEX_POINT('',#11253);
#2818=VERTEX_POINT('',#11254);
#2819=VERTEX_POINT('',#11278);
#2820=VERTEX_POINT('',#11279);
#2821=VERTEX_POINT('',#11303);
#2822=VERTEX_POINT('',#11304);
#2823=VERTEX_POINT('',#11327);
#2824=VERTEX_POINT('',#11328);
#2825=VERTEX_POINT('',#11352);
#2826=VERTEX_POINT('',#11353);
#2827=VERTEX_POINT('',#11377);
#2828=VERTEX_POINT('',#11378);
#2829=VERTEX_POINT('',#11380);
#2830=VERTEX_POINT('',#11386);
#2831=VERTEX_POINT('',#11394);
#2832=VERTEX_POINT('',#11396);
#2833=VERTEX_POINT('',#11400);
#2834=VERTEX_POINT('',#11402);
#2835=VERTEX_POINT('',#11407);
#2836=VERTEX_POINT('',#11408);
#2837=VERTEX_POINT('',#11410);
#2838=VERTEX_POINT('',#11412);
#2839=VERTEX_POINT('',#11414);
#2840=VERTEX_POINT('',#11417);
#2841=VERTEX_POINT('',#11418);
#2842=VERTEX_POINT('',#11420);
#2843=VERTEX_POINT('',#11422);
#2844=VERTEX_POINT('',#11425);
#2845=VERTEX_POINT('',#11426);
#2846=VERTEX_POINT('',#11428);
#2847=VERTEX_POINT('',#11430);
#2848=VERTEX_POINT('',#11433);
#2849=VERTEX_POINT('',#12188);
#2850=VERTEX_POINT('',#12190);
#2851=VERTEX_POINT('',#14453);
#2852=VERTEX_POINT('',#14455);
#2853=VERTEX_POINT('',#14459);
#2854=VERTEX_POINT('',#14461);
#2855=VERTEX_POINT('',#14465);
#2856=VERTEX_POINT('',#14467);
#2857=VERTEX_POINT('',#14471);
#2858=VERTEX_POINT('',#14473);
#2859=VERTEX_POINT('',#14477);
#2860=VERTEX_POINT('',#14479);
#2861=VERTEX_POINT('',#14482);
#2862=VERTEX_POINT('',#14486);
#2863=VERTEX_POINT('',#14491);
#2864=VERTEX_POINT('',#14493);
#2865=VERTEX_POINT('',#14497);
#2866=VERTEX_POINT('',#14499);
#2867=VERTEX_POINT('',#14503);
#2868=VERTEX_POINT('',#14505);
#2869=VERTEX_POINT('',#14509);
#2870=VERTEX_POINT('',#14511);
#2871=VERTEX_POINT('',#14515);
#2872=VERTEX_POINT('',#14517);
#2873=VERTEX_POINT('',#14524);
#2874=VERTEX_POINT('',#14528);
#2875=VERTEX_POINT('',#14531);
#2876=VERTEX_POINT('',#14542);
#2877=VERTEX_POINT('',#14629);
#2878=VERTEX_POINT('',#14634);
#2879=VERTEX_POINT('',#14636);
#2880=VERTEX_POINT('',#14638);
#2881=VERTEX_POINT('',#14640);
#2882=VERTEX_POINT('',#14642);
#2883=VERTEX_POINT('',#14644);
#2884=VERTEX_POINT('',#14647);
#2885=VERTEX_POINT('',#14651);
#2886=VERTEX_POINT('',#14655);
#2887=VERTEX_POINT('',#14659);
#2888=VERTEX_POINT('',#14663);
#2889=VERTEX_POINT('',#14665);
#2890=VERTEX_POINT('',#14670);
#2891=VERTEX_POINT('',#14671);
#2892=VERTEX_POINT('',#14674);
#2893=VERTEX_POINT('',#14679);
#2894=VERTEX_POINT('',#14681);
#2895=VERTEX_POINT('',#14751);
#2896=VERTEX_POINT('',#14753);
#2897=VERTEX_POINT('',#14811);
#2898=VERTEX_POINT('',#14813);
#2899=VERTEX_POINT('',#14818);
#2900=VERTEX_POINT('',#14820);
#2901=VERTEX_POINT('',#14824);
#2902=VERTEX_POINT('',#14826);
#2903=VERTEX_POINT('',#14830);
#2904=VERTEX_POINT('',#14832);
#2905=VERTEX_POINT('',#14836);
#2906=VERTEX_POINT('',#14838);
#2907=VERTEX_POINT('',#14842);
#2908=VERTEX_POINT('',#14844);
#2909=VERTEX_POINT('',#14848);
#2910=VERTEX_POINT('',#14850);
#2911=VERTEX_POINT('',#14854);
#2912=VERTEX_POINT('',#14857);
#2913=VERTEX_POINT('',#14859);
#2914=VERTEX_POINT('',#14862);
#2915=VERTEX_POINT('',#14866);
#2916=VERTEX_POINT('',#14872);
#2917=VERTEX_POINT('',#14879);
#2918=VERTEX_POINT('',#14880);
#2919=VERTEX_POINT('',#14882);
#2920=VERTEX_POINT('',#14884);
#2921=VERTEX_POINT('',#14897);
#2922=VERTEX_POINT('',#14908);
#2923=VERTEX_POINT('',#14913);
#2924=VERTEX_POINT('',#14915);
#2925=VERTEX_POINT('',#14919);
#2926=VERTEX_POINT('',#14938);
#2927=VERTEX_POINT('',#14946);
#2928=VERTEX_POINT('',#14949);
#2929=VERTEX_POINT('',#14953);
#2930=VERTEX_POINT('',#14954);
#2931=VERTEX_POINT('',#14956);
#2932=VERTEX_POINT('',#14958);
#2933=VERTEX_POINT('',#14962);
#2934=VERTEX_POINT('',#14981);
#2935=VERTEX_POINT('',#14985);
#2936=VERTEX_POINT('',#14987);
#2937=VERTEX_POINT('',#15012);
#2938=VERTEX_POINT('',#15013);
#2939=VERTEX_POINT('',#15015);
#2940=VERTEX_POINT('',#15017);
#2941=VERTEX_POINT('',#15021);
#2942=VERTEX_POINT('',#15040);
#2943=VERTEX_POINT('',#15044);
#2944=VERTEX_POINT('',#15046);
#2945=VERTEX_POINT('',#15071);
#2946=VERTEX_POINT('',#15073);
#2947=VERTEX_POINT('',#15077);
#2948=VERTEX_POINT('',#15081);
#2949=VERTEX_POINT('',#15083);
#2950=VERTEX_POINT('',#15086);
#2951=VERTEX_POINT('',#15088);
#2952=VERTEX_POINT('',#15093);
#2953=VERTEX_POINT('',#15102);
#2954=VERTEX_POINT('',#15104);
#2955=VERTEX_POINT('',#15108);
#2956=VERTEX_POINT('',#15110);
#2957=VERTEX_POINT('',#15117);
#2958=VERTEX_POINT('',#15119);
#2959=VERTEX_POINT('',#15123);
#2960=VERTEX_POINT('',#15125);
#2961=VERTEX_POINT('',#15132);
#2962=VERTEX_POINT('',#15134);
#2963=VERTEX_POINT('',#15138);
#2964=VERTEX_POINT('',#15140);
#2965=VERTEX_POINT('',#15147);
#2966=VERTEX_POINT('',#15149);
#2967=VERTEX_POINT('',#15153);
#2968=VERTEX_POINT('',#15155);
#2969=VERTEX_POINT('',#15162);
#2970=VERTEX_POINT('',#15163);
#2971=VERTEX_POINT('',#15165);
#2972=VERTEX_POINT('',#15167);
#2973=VERTEX_POINT('',#15171);
#2974=VERTEX_POINT('',#15173);
#2975=VERTEX_POINT('',#15177);
#2976=VERTEX_POINT('',#15179);
#2977=VERTEX_POINT('',#15189);
#2978=VERTEX_POINT('',#15191);
#2979=VERTEX_POINT('',#15195);
#2980=VERTEX_POINT('',#15197);
#2981=VERTEX_POINT('',#15204);
#2982=VERTEX_POINT('',#15206);
#2983=VERTEX_POINT('',#15210);
#2984=VERTEX_POINT('',#15212);
#2985=VERTEX_POINT('',#15219);
#2986=VERTEX_POINT('',#15221);
#2987=VERTEX_POINT('',#15225);
#2988=VERTEX_POINT('',#15227);
#2989=VERTEX_POINT('',#15234);
#2990=VERTEX_POINT('',#15236);
#2991=VERTEX_POINT('',#15240);
#2992=VERTEX_POINT('',#15242);
#2993=VERTEX_POINT('',#15249);
#2994=VERTEX_POINT('',#15250);
#2995=VERTEX_POINT('',#15252);
#2996=VERTEX_POINT('',#15254);
#2997=VERTEX_POINT('',#15258);
#2998=VERTEX_POINT('',#15259);
#2999=VERTEX_POINT('',#15261);
#3000=VERTEX_POINT('',#15263);
#3001=VERTEX_POINT('',#15276);
#3002=VERTEX_POINT('',#15277);
#3003=VERTEX_POINT('',#15279);
#3004=VERTEX_POINT('',#15290);
#3005=VERTEX_POINT('',#15292);
#3006=VERTEX_POINT('',#15295);
#3007=VERTEX_POINT('',#15305);
#3008=VERTEX_POINT('',#15306);
#3009=VERTEX_POINT('',#15353);
#3010=VERTEX_POINT('',#15354);
#3011=VERTEX_POINT('',#15401);
#3012=VERTEX_POINT('',#15402);
#3013=VERTEX_POINT('',#15449);
#3014=VERTEX_POINT('',#15450);
#3015=VERTEX_POINT('',#15503);
#3016=VERTEX_POINT('',#15504);
#3017=VERTEX_POINT('',#15551);
#3018=VERTEX_POINT('',#15552);
#3019=VERTEX_POINT('',#15599);
#3020=VERTEX_POINT('',#15600);
#3021=VERTEX_POINT('',#15602);
#3022=VERTEX_POINT('',#15613);
#3023=VERTEX_POINT('',#15624);
#3024=VERTEX_POINT('',#15625);
#3025=VERTEX_POINT('',#15649);
#3026=VERTEX_POINT('',#15650);
#3027=VERTEX_POINT('',#15673);
#3028=VERTEX_POINT('',#15674);
#3029=VERTEX_POINT('',#15698);
#3030=VERTEX_POINT('',#15699);
#3031=VERTEX_POINT('',#15723);
#3032=VERTEX_POINT('',#15724);
#3033=VERTEX_POINT('',#15747);
#3034=VERTEX_POINT('',#15748);
#3035=VERTEX_POINT('',#15771);
#3036=VERTEX_POINT('',#15911);
#3037=VERTEX_POINT('',#15952);
#3038=VERTEX_POINT('',#15973);
#3039=VERTEX_POINT('',#16180);
#3040=VERTEX_POINT('',#16267);
#3041=VERTEX_POINT('',#16570);
#3042=VERTEX_POINT('',#16571);
#3043=VERTEX_POINT('',#16573);
#3044=VERTEX_POINT('',#16575);
#3045=VERTEX_POINT('',#16579);
#3046=VERTEX_POINT('',#16581);
#3047=VERTEX_POINT('',#16585);
#3048=VERTEX_POINT('',#16587);
#3049=VERTEX_POINT('',#16591);
#3050=VERTEX_POINT('',#16593);
#3051=VERTEX_POINT('',#16597);
#3052=VERTEX_POINT('',#16599);
#3053=VERTEX_POINT('',#16607);
#3054=VERTEX_POINT('',#16610);
#3055=EDGE_CURVE('',#2499,#2499,#2240,.T.);
#3056=EDGE_CURVE('',#2499,#2500,#1502,.T.);
#3057=EDGE_CURVE('',#2500,#2500,#2241,.T.);
#3058=EDGE_CURVE('',#2501,#2501,#2242,.T.);
#3059=EDGE_CURVE('',#2501,#2502,#1503,.T.);
#3060=EDGE_CURVE('',#2502,#2502,#2243,.T.);
#3061=EDGE_CURVE('',#2503,#2503,#2244,.T.);
#3062=EDGE_CURVE('',#2504,#2504,#2245,.T.);
#3063=EDGE_CURVE('',#2504,#2505,#1504,.T.);
#3064=EDGE_CURVE('',#2505,#2505,#2246,.T.);
#3065=EDGE_CURVE('',#2506,#2506,#2247,.T.);
#3066=EDGE_CURVE('',#2506,#2507,#1505,.T.);
#3067=EDGE_CURVE('',#2507,#2507,#2248,.T.);
#3068=EDGE_CURVE('',#2508,#2508,#2249,.T.);
#3069=EDGE_CURVE('',#2508,#2509,#1506,.T.);
#3070=EDGE_CURVE('',#2509,#2509,#2250,.T.);
#3071=EDGE_CURVE('',#2510,#2510,#2251,.T.);
#3072=EDGE_CURVE('',#2510,#2511,#1507,.T.);
#3073=EDGE_CURVE('',#2511,#2511,#2252,.T.);
#3074=EDGE_CURVE('',#2512,#2513,#1508,.T.);
#3075=EDGE_CURVE('',#2512,#2514,#1509,.T.);
#3076=EDGE_CURVE('',#2515,#2514,#1510,.T.);
#3077=EDGE_CURVE('',#2513,#2515,#1511,.T.);
#3078=EDGE_CURVE('',#2513,#2516,#2253,.T.);
#3079=EDGE_CURVE('',#2517,#2515,#2254,.T.);
#3080=EDGE_CURVE('',#2516,#2517,#1512,.T.);
#3081=EDGE_CURVE('',#2516,#2518,#1513,.T.);
#3082=EDGE_CURVE('',#2519,#2517,#1514,.T.);
#3083=EDGE_CURVE('',#2518,#2519,#1515,.T.);
#3084=EDGE_CURVE('',#2518,#2512,#2255,.T.);
#3085=EDGE_CURVE('',#2514,#2519,#2256,.T.);
#3086=EDGE_CURVE('',#2520,#2521,#1516,.T.);
#3087=EDGE_CURVE('',#2520,#2522,#1517,.T.);
#3088=EDGE_CURVE('',#2523,#2522,#1518,.T.);
#3089=EDGE_CURVE('',#2521,#2523,#1519,.T.);
#3090=EDGE_CURVE('',#2521,#2524,#2257,.T.);
#3091=EDGE_CURVE('',#2525,#2523,#2258,.T.);
#3092=EDGE_CURVE('',#2524,#2525,#1520,.T.);
#3093=EDGE_CURVE('',#2524,#2526,#1521,.T.);
#3094=EDGE_CURVE('',#2527,#2525,#1522,.T.);
#3095=EDGE_CURVE('',#2526,#2527,#1523,.T.);
#3096=EDGE_CURVE('',#2526,#2520,#2259,.T.);
#3097=EDGE_CURVE('',#2522,#2527,#2260,.T.);
#3098=EDGE_CURVE('',#2528,#2529,#1524,.T.);
#3099=EDGE_CURVE('',#2528,#2530,#1525,.T.);
#3100=EDGE_CURVE('',#2531,#2530,#1526,.T.);
#3101=EDGE_CURVE('',#2529,#2531,#1527,.T.);
#3102=EDGE_CURVE('',#2529,#2532,#2261,.T.);
#3103=EDGE_CURVE('',#2533,#2531,#2262,.T.);
#3104=EDGE_CURVE('',#2532,#2533,#1528,.T.);
#3105=EDGE_CURVE('',#2532,#2534,#1529,.T.);
#3106=EDGE_CURVE('',#2535,#2533,#1530,.T.);
#3107=EDGE_CURVE('',#2534,#2535,#1531,.T.);
#3108=EDGE_CURVE('',#2534,#2528,#2263,.T.);
#3109=EDGE_CURVE('',#2530,#2535,#2264,.T.);
#3110=EDGE_CURVE('',#2536,#2537,#1532,.T.);
#3111=EDGE_CURVE('',#2536,#2538,#1533,.T.);
#3112=EDGE_CURVE('',#2539,#2538,#1534,.T.);
#3113=EDGE_CURVE('',#2537,#2539,#1535,.T.);
#3114=EDGE_CURVE('',#2537,#2540,#2265,.T.);
#3115=EDGE_CURVE('',#2541,#2539,#2266,.T.);
#3116=EDGE_CURVE('',#2540,#2541,#1536,.T.);
#3117=EDGE_CURVE('',#2540,#2542,#1537,.T.);
#3118=EDGE_CURVE('',#2543,#2541,#1538,.T.);
#3119=EDGE_CURVE('',#2542,#2543,#1539,.T.);
#3120=EDGE_CURVE('',#2542,#2536,#2267,.T.);
#3121=EDGE_CURVE('',#2538,#2543,#2268,.T.);
#3122=EDGE_CURVE('',#2544,#2545,#1540,.T.);
#3123=EDGE_CURVE('',#2544,#2546,#1541,.T.);
#3124=EDGE_CURVE('',#2547,#2546,#1542,.T.);
#3125=EDGE_CURVE('',#2545,#2547,#1543,.T.);
#3126=EDGE_CURVE('',#2545,#2548,#2269,.T.);
#3127=EDGE_CURVE('',#2549,#2547,#2270,.T.);
#3128=EDGE_CURVE('',#2548,#2549,#1544,.T.);
#3129=EDGE_CURVE('',#2548,#2550,#1545,.T.);
#3130=EDGE_CURVE('',#2551,#2549,#1546,.T.);
#3131=EDGE_CURVE('',#2550,#2551,#1547,.T.);
#3132=EDGE_CURVE('',#2550,#2544,#2271,.T.);
#3133=EDGE_CURVE('',#2546,#2551,#2272,.T.);
#3134=EDGE_CURVE('',#2552,#2553,#1548,.T.);
#3135=EDGE_CURVE('',#2552,#2554,#1549,.T.);
#3136=EDGE_CURVE('',#2555,#2554,#1550,.T.);
#3137=EDGE_CURVE('',#2553,#2555,#1551,.T.);
#3138=EDGE_CURVE('',#2553,#2556,#2273,.T.);
#3139=EDGE_CURVE('',#2557,#2555,#2274,.T.);
#3140=EDGE_CURVE('',#2556,#2557,#1552,.T.);
#3141=EDGE_CURVE('',#2556,#2558,#1553,.T.);
#3142=EDGE_CURVE('',#2559,#2557,#1554,.T.);
#3143=EDGE_CURVE('',#2558,#2559,#1555,.T.);
#3144=EDGE_CURVE('',#2558,#2552,#2275,.T.);
#3145=EDGE_CURVE('',#2554,#2559,#2276,.T.);
#3146=EDGE_CURVE('',#2560,#2561,#1556,.T.);
#3147=EDGE_CURVE('',#2562,#2560,#1557,.T.);
#3148=EDGE_CURVE('',#2563,#2562,#1558,.T.);
#3149=EDGE_CURVE('',#2563,#2561,#1559,.T.);
#3150=EDGE_CURVE('',#2564,#2565,#1560,.T.);
#3151=EDGE_CURVE('',#2564,#2566,#1561,.T.);
#3152=EDGE_CURVE('',#2567,#2566,#1562,.T.);
#3153=EDGE_CURVE('',#2565,#2567,#1563,.T.);
#3154=EDGE_CURVE('',#2568,#2569,#1564,.T.);
#3155=EDGE_CURVE('',#2570,#2568,#1565,.T.);
#3156=EDGE_CURVE('',#2571,#2570,#1566,.T.);
#3157=EDGE_CURVE('',#2571,#2569,#1567,.T.);
#3158=EDGE_CURVE('',#2572,#2573,#1568,.T.);
#3159=EDGE_CURVE('',#2572,#2574,#1569,.T.);
#3160=EDGE_CURVE('',#2575,#2574,#1570,.T.);
#3161=EDGE_CURVE('',#2573,#2575,#1571,.T.);
#3162=EDGE_CURVE('',#2569,#2564,#2277,.T.);
#3163=EDGE_CURVE('',#2574,#2571,#2278,.T.);
#3164=EDGE_CURVE('',#2576,#2572,#2279,.T.);
#3165=EDGE_CURVE('',#2577,#2576,#1572,.T.);
#3166=EDGE_CURVE('',#2578,#2577,#2280,.T.);
#3167=EDGE_CURVE('',#2579,#2578,#1573,.T.);
#3168=EDGE_CURVE('',#2561,#2579,#2281,.T.);
#3169=EDGE_CURVE('',#2566,#2563,#2282,.T.);
#3170=EDGE_CURVE('',#2580,#2580,#2283,.T.);
#3171=EDGE_CURVE('',#2581,#2573,#2284,.T.);
#3172=EDGE_CURVE('',#2576,#2581,#1574,.T.);
#3173=EDGE_CURVE('',#2568,#2565,#2285,.T.);
#3174=EDGE_CURVE('',#2582,#2579,#1575,.T.);
#3175=EDGE_CURVE('',#2560,#2582,#2286,.T.);
#3176=EDGE_CURVE('',#2583,#2583,#2287,.T.);
#3177=EDGE_CURVE('',#2583,#2580,#1576,.T.);
#3178=EDGE_CURVE('',#2582,#2584,#1577,.T.);
#3179=EDGE_CURVE('',#2585,#2584,#2288,.T.);
#3180=EDGE_CURVE('',#2585,#2581,#1578,.T.);
#3181=EDGE_CURVE('',#2570,#2575,#2289,.T.);
#3182=EDGE_CURVE('',#2562,#2567,#2290,.T.);
#3183=EDGE_CURVE('',#2584,#2578,#1579,.T.);
#3184=EDGE_CURVE('',#2577,#2585,#1580,.T.);
#3185=EDGE_CURVE('',#2503,#2586,#1581,.T.);
#3186=EDGE_CURVE('',#2586,#2586,#2291,.T.);
#3187=EDGE_CURVE('',#2587,#2587,#2292,.T.);
#3188=EDGE_CURVE('',#2587,#2588,#1582,.T.);
#3189=EDGE_CURVE('',#2588,#2588,#2293,.T.);
#3190=EDGE_CURVE('',#2589,#2589,#2294,.T.);
#3191=EDGE_CURVE('',#2589,#2590,#1583,.T.);
#3192=EDGE_CURVE('',#2590,#2590,#2295,.T.);
#3193=EDGE_CURVE('',#2591,#2591,#2296,.T.);
#3194=EDGE_CURVE('',#2591,#2592,#1584,.T.);
#3195=EDGE_CURVE('',#2592,#2592,#2297,.T.);
#3196=EDGE_CURVE('',#2593,#2593,#2298,.T.);
#3197=EDGE_CURVE('',#2594,#2594,#2299,.T.);
#3198=EDGE_CURVE('',#2594,#2595,#1585,.T.);
#3199=EDGE_CURVE('',#2595,#2595,#2300,.T.);
#3200=EDGE_CURVE('',#2596,#2596,#2301,.T.);
#3201=EDGE_CURVE('',#2596,#2597,#1586,.T.);
#3202=EDGE_CURVE('',#2597,#2597,#2302,.T.);
#3203=EDGE_CURVE('',#2598,#2598,#2303,.T.);
#3204=EDGE_CURVE('',#2598,#2599,#1587,.T.);
#3205=EDGE_CURVE('',#2599,#2599,#2304,.T.);
#3206=EDGE_CURVE('',#2600,#2600,#2305,.T.);
#3207=EDGE_CURVE('',#2600,#2601,#1588,.T.);
#3208=EDGE_CURVE('',#2601,#2601,#2306,.T.);
#3209=EDGE_CURVE('',#2593,#2602,#1589,.T.);
#3210=EDGE_CURVE('',#2602,#2602,#2307,.T.);
#3211=EDGE_CURVE('',#2603,#2603,#2308,.T.);
#3212=EDGE_CURVE('',#2603,#2604,#1590,.T.);
#3213=EDGE_CURVE('',#2604,#2604,#2309,.T.);
#3214=EDGE_CURVE('',#2605,#2606,#1591,.T.);
#3215=EDGE_CURVE('',#2605,#2607,#1592,.T.);
#3216=EDGE_CURVE('',#2607,#2608,#1593,.T.);
#3217=EDGE_CURVE('',#2606,#2608,#1594,.T.);
#3218=EDGE_CURVE('',#2607,#2609,#1595,.T.);
#3219=EDGE_CURVE('',#2609,#2610,#1596,.T.);
#3220=EDGE_CURVE('',#2608,#2610,#1597,.T.);
#3221=EDGE_CURVE('',#2611,#2612,#1598,.T.);
#3222=EDGE_CURVE('',#2610,#2611,#1599,.T.);
#3223=EDGE_CURVE('',#2609,#2612,#1600,.T.);
#3224=EDGE_CURVE('',#2612,#2605,#2310,.T.);
#3225=EDGE_CURVE('',#2613,#2613,#2311,.T.);
#3226=EDGE_CURVE('',#2614,#2615,#2312,.T.);
#3227=EDGE_CURVE('',#2615,#2616,#1601,.T.);
#3228=EDGE_CURVE('',#2616,#2617,#2313,.T.);
#3229=EDGE_CURVE('',#2617,#2614,#1602,.T.);
#3230=EDGE_CURVE('',#2618,#2619,#2314,.T.);
#3231=EDGE_CURVE('',#2619,#2620,#1603,.T.);
#3232=EDGE_CURVE('',#2620,#2621,#2315,.T.);
#3233=EDGE_CURVE('',#2621,#2618,#1604,.T.);
#3234=EDGE_CURVE('',#2622,#2623,#2316,.T.);
#3235=EDGE_CURVE('',#2623,#2624,#1605,.T.);
#3236=EDGE_CURVE('',#2624,#2625,#2317,.T.);
#3237=EDGE_CURVE('',#2625,#2622,#1606,.T.);
#3238=EDGE_CURVE('',#2626,#2627,#2318,.T.);
#3239=EDGE_CURVE('',#2627,#2628,#1607,.T.);
#3240=EDGE_CURVE('',#2628,#2629,#2319,.T.);
#3241=EDGE_CURVE('',#2629,#2626,#1608,.T.);
#3242=EDGE_CURVE('',#2630,#2631,#2320,.T.);
#3243=EDGE_CURVE('',#2631,#2632,#1609,.T.);
#3244=EDGE_CURVE('',#2632,#2633,#2321,.T.);
#3245=EDGE_CURVE('',#2633,#2630,#1610,.T.);
#3246=EDGE_CURVE('',#2634,#2635,#2322,.T.);
#3247=EDGE_CURVE('',#2635,#2636,#1611,.T.);
#3248=EDGE_CURVE('',#2636,#2637,#2323,.T.);
#3249=EDGE_CURVE('',#2637,#2634,#1612,.T.);
#3250=EDGE_CURVE('',#2638,#2611,#2324,.T.);
#3251=EDGE_CURVE('',#2606,#2638,#2325,.T.);
#3252=EDGE_CURVE('',#2639,#2640,#2326,.T.);
#3253=EDGE_CURVE('',#2639,#2615,#1613,.T.);
#3254=EDGE_CURVE('',#2640,#2614,#1614,.T.);
#3255=EDGE_CURVE('',#2641,#2640,#1615,.T.);
#3256=EDGE_CURVE('',#2641,#2617,#1616,.T.);
#3257=EDGE_CURVE('',#2642,#2641,#2327,.T.);
#3258=EDGE_CURVE('',#2642,#2616,#1617,.T.);
#3259=EDGE_CURVE('',#2639,#2642,#1618,.T.);
#3260=EDGE_CURVE('',#2643,#2644,#2328,.T.);
#3261=EDGE_CURVE('',#2643,#2619,#1619,.T.);
#3262=EDGE_CURVE('',#2644,#2618,#1620,.T.);
#3263=EDGE_CURVE('',#2645,#2644,#1621,.T.);
#3264=EDGE_CURVE('',#2645,#2621,#1622,.T.);
#3265=EDGE_CURVE('',#2646,#2645,#2329,.T.);
#3266=EDGE_CURVE('',#2646,#2620,#1623,.T.);
#3267=EDGE_CURVE('',#2643,#2646,#1624,.T.);
#3268=EDGE_CURVE('',#2647,#2648,#2330,.T.);
#3269=EDGE_CURVE('',#2647,#2623,#1625,.T.);
#3270=EDGE_CURVE('',#2648,#2622,#1626,.T.);
#3271=EDGE_CURVE('',#2649,#2648,#1627,.T.);
#3272=EDGE_CURVE('',#2649,#2625,#1628,.T.);
#3273=EDGE_CURVE('',#2650,#2649,#2331,.T.);
#3274=EDGE_CURVE('',#2650,#2624,#1629,.T.);
#3275=EDGE_CURVE('',#2647,#2650,#1630,.T.);
#3276=EDGE_CURVE('',#2651,#2652,#2332,.T.);
#3277=EDGE_CURVE('',#2651,#2627,#1631,.T.);
#3278=EDGE_CURVE('',#2652,#2626,#1632,.T.);
#3279=EDGE_CURVE('',#2653,#2652,#1633,.T.);
#3280=EDGE_CURVE('',#2653,#2629,#1634,.T.);
#3281=EDGE_CURVE('',#2654,#2653,#2333,.T.);
#3282=EDGE_CURVE('',#2654,#2628,#1635,.T.);
#3283=EDGE_CURVE('',#2651,#2654,#1636,.T.);
#3284=EDGE_CURVE('',#2655,#2656,#2334,.T.);
#3285=EDGE_CURVE('',#2655,#2631,#1637,.T.);
#3286=EDGE_CURVE('',#2656,#2630,#1638,.T.);
#3287=EDGE_CURVE('',#2657,#2656,#1639,.T.);
#3288=EDGE_CURVE('',#2657,#2633,#1640,.T.);
#3289=EDGE_CURVE('',#2658,#2657,#2335,.T.);
#3290=EDGE_CURVE('',#2658,#2632,#1641,.T.);
#3291=EDGE_CURVE('',#2655,#2658,#1642,.T.);
#3292=EDGE_CURVE('',#2659,#2660,#2336,.T.);
#3293=EDGE_CURVE('',#2659,#2635,#1643,.T.);
#3294=EDGE_CURVE('',#2660,#2634,#1644,.T.);
#3295=EDGE_CURVE('',#2661,#2660,#1645,.T.);
#3296=EDGE_CURVE('',#2661,#2637,#1646,.T.);
#3297=EDGE_CURVE('',#2662,#2661,#2337,.T.);
#3298=EDGE_CURVE('',#2662,#2636,#1647,.T.);
#3299=EDGE_CURVE('',#2659,#2662,#1648,.T.);
#3300=EDGE_CURVE('',#2663,#2663,#2338,.T.);
#3301=EDGE_CURVE('',#2663,#2664,#1649,.T.);
#3302=EDGE_CURVE('',#2664,#2664,#2339,.T.);
#3303=EDGE_CURVE('',#2665,#2665,#2340,.T.);
#3304=EDGE_CURVE('',#2665,#2638,#1650,.T.);
#3305=EDGE_CURVE('',#2666,#2666,#2341,.T.);
#3306=EDGE_CURVE('',#2666,#2613,#1651,.T.);
#3307=EDGE_CURVE('',#2667,#2667,#2342,.T.);
#3308=EDGE_CURVE('',#2667,#2668,#1652,.T.);
#3309=EDGE_CURVE('',#2668,#2668,#2343,.T.);
#3310=EDGE_CURVE('',#2669,#2669,#2344,.T.);
#3311=EDGE_CURVE('',#2669,#2670,#1653,.T.);
#3312=EDGE_CURVE('',#2670,#2670,#2345,.T.);
#3313=EDGE_CURVE('',#2671,#2672,#1654,.T.);
#3314=EDGE_CURVE('',#2672,#2673,#148,.T.);
#3315=EDGE_CURVE('',#2674,#2673,#2346,.F.);
#3316=EDGE_CURVE('',#2674,#2671,#149,.T.);
#3317=EDGE_CURVE('',#2675,#2676,#1655,.T.);
#3318=EDGE_CURVE('',#2676,#2672,#150,.T.);
#3319=EDGE_CURVE('',#2671,#2675,#151,.T.);
#3320=EDGE_CURVE('',#2677,#2678,#1656,.T.);
#3321=EDGE_CURVE('',#2678,#2676,#152,.T.);
#3322=EDGE_CURVE('',#2675,#2677,#153,.T.);
#3323=EDGE_CURVE('',#2679,#2680,#1657,.T.);
#3324=EDGE_CURVE('',#2680,#2678,#154,.T.);
#3325=EDGE_CURVE('',#2677,#2679,#155,.T.);
#3326=EDGE_CURVE('',#2681,#2682,#1658,.T.);
#3327=EDGE_CURVE('',#2682,#2680,#156,.T.);
#3328=EDGE_CURVE('',#2679,#2681,#157,.T.);
#3329=EDGE_CURVE('',#2683,#2684,#1659,.T.);
#3330=EDGE_CURVE('',#2684,#2682,#158,.T.);
#3331=EDGE_CURVE('',#2681,#2683,#159,.T.);
#3332=EDGE_CURVE('',#2685,#2686,#1660,.T.);
#3333=EDGE_CURVE('',#2686,#2684,#160,.T.);
#3334=EDGE_CURVE('',#2683,#2685,#161,.T.);
#3335=EDGE_CURVE('',#2687,#2688,#1661,.T.);
#3336=EDGE_CURVE('',#2687,#2689,#162,.T.);
#3337=EDGE_CURVE('',#2690,#2689,#2347,.T.);
#3338=EDGE_CURVE('',#2690,#2688,#163,.T.);
#3339=EDGE_CURVE('',#2691,#2692,#1662,.T.);
#3340=EDGE_CURVE('',#2692,#2693,#164,.T.);
#3341=EDGE_CURVE('',#2694,#2693,#2348,.F.);
#3342=EDGE_CURVE('',#2694,#2691,#165,.T.);
#3343=EDGE_CURVE('',#2695,#2696,#1663,.T.);
#3344=EDGE_CURVE('',#2696,#2692,#166,.T.);
#3345=EDGE_CURVE('',#2691,#2695,#167,.T.);
#3346=EDGE_CURVE('',#2697,#2698,#1664,.T.);
#3347=EDGE_CURVE('',#2698,#2696,#168,.T.);
#3348=EDGE_CURVE('',#2695,#2697,#169,.T.);
#3349=EDGE_CURVE('',#2699,#2700,#1665,.T.);
#3350=EDGE_CURVE('',#2700,#2698,#170,.T.);
#3351=EDGE_CURVE('',#2697,#2699,#171,.T.);
#3352=EDGE_CURVE('',#2701,#2702,#1666,.T.);
#3353=EDGE_CURVE('',#2702,#2700,#172,.T.);
#3354=EDGE_CURVE('',#2699,#2701,#173,.T.);
#3355=EDGE_CURVE('',#2703,#2704,#1667,.T.);
#3356=EDGE_CURVE('',#2704,#2702,#174,.T.);
#3357=EDGE_CURVE('',#2701,#2703,#175,.T.);
#3358=EDGE_CURVE('',#2705,#2706,#1668,.T.);
#3359=EDGE_CURVE('',#2706,#2704,#176,.T.);
#3360=EDGE_CURVE('',#2703,#2705,#177,.T.);
#3361=EDGE_CURVE('',#2707,#2708,#1669,.T.);
#3362=EDGE_CURVE('',#2707,#2709,#178,.T.);
#3363=EDGE_CURVE('',#2710,#2709,#2349,.T.);
#3364=EDGE_CURVE('',#2710,#2708,#179,.T.);
#3365=EDGE_CURVE('',#2711,#2712,#1670,.T.);
#3366=EDGE_CURVE('',#2712,#2713,#180,.T.);
#3367=EDGE_CURVE('',#2714,#2713,#2350,.F.);
#3368=EDGE_CURVE('',#2714,#2711,#181,.T.);
#3369=EDGE_CURVE('',#2715,#2716,#1671,.T.);
#3370=EDGE_CURVE('',#2716,#2712,#182,.T.);
#3371=EDGE_CURVE('',#2711,#2715,#183,.T.);
#3372=EDGE_CURVE('',#2717,#2718,#1672,.T.);
#3373=EDGE_CURVE('',#2718,#2716,#184,.T.);
#3374=EDGE_CURVE('',#2715,#2717,#185,.T.);
#3375=EDGE_CURVE('',#2719,#2720,#1673,.T.);
#3376=EDGE_CURVE('',#2720,#2718,#186,.T.);
#3377=EDGE_CURVE('',#2717,#2719,#187,.T.);
#3378=EDGE_CURVE('',#2721,#2722,#1674,.T.);
#3379=EDGE_CURVE('',#2722,#2720,#188,.T.);
#3380=EDGE_CURVE('',#2719,#2721,#189,.T.);
#3381=EDGE_CURVE('',#2723,#2724,#1675,.T.);
#3382=EDGE_CURVE('',#2724,#2722,#190,.T.);
#3383=EDGE_CURVE('',#2721,#2723,#191,.T.);
#3384=EDGE_CURVE('',#2725,#2726,#1676,.T.);
#3385=EDGE_CURVE('',#2726,#2724,#192,.T.);
#3386=EDGE_CURVE('',#2723,#2725,#193,.T.);
#3387=EDGE_CURVE('',#2727,#2728,#1677,.T.);
#3388=EDGE_CURVE('',#2727,#2729,#194,.T.);
#3389=EDGE_CURVE('',#2730,#2729,#2351,.T.);
#3390=EDGE_CURVE('',#2730,#2728,#195,.T.);
#3391=EDGE_CURVE('',#2731,#2732,#1678,.T.);
#3392=EDGE_CURVE('',#2732,#2733,#196,.T.);
#3393=EDGE_CURVE('',#2734,#2733,#2352,.F.);
#3394=EDGE_CURVE('',#2734,#2731,#197,.T.);
#3395=EDGE_CURVE('',#2735,#2736,#1679,.T.);
#3396=EDGE_CURVE('',#2736,#2732,#198,.T.);
#3397=EDGE_CURVE('',#2731,#2735,#199,.T.);
#3398=EDGE_CURVE('',#2737,#2738,#1680,.T.);
#3399=EDGE_CURVE('',#2738,#2736,#200,.T.);
#3400=EDGE_CURVE('',#2735,#2737,#201,.T.);
#3401=EDGE_CURVE('',#2739,#2740,#1681,.T.);
#3402=EDGE_CURVE('',#2740,#2738,#202,.T.);
#3403=EDGE_CURVE('',#2737,#2739,#203,.T.);
#3404=EDGE_CURVE('',#2741,#2742,#1682,.T.);
#3405=EDGE_CURVE('',#2742,#2740,#204,.T.);
#3406=EDGE_CURVE('',#2739,#2741,#205,.T.);
#3407=EDGE_CURVE('',#2743,#2744,#1683,.T.);
#3408=EDGE_CURVE('',#2744,#2742,#206,.T.);
#3409=EDGE_CURVE('',#2741,#2743,#207,.T.);
#3410=EDGE_CURVE('',#2745,#2746,#1684,.T.);
#3411=EDGE_CURVE('',#2746,#2744,#208,.T.);
#3412=EDGE_CURVE('',#2743,#2745,#209,.T.);
#3413=EDGE_CURVE('',#2747,#2748,#1685,.T.);
#3414=EDGE_CURVE('',#2747,#2749,#210,.T.);
#3415=EDGE_CURVE('',#2750,#2749,#2353,.T.);
#3416=EDGE_CURVE('',#2750,#2748,#211,.T.);
#3417=EDGE_CURVE('',#2751,#2752,#1686,.T.);
#3418=EDGE_CURVE('',#2752,#2753,#212,.T.);
#3419=EDGE_CURVE('',#2754,#2753,#2354,.T.);
#3420=EDGE_CURVE('',#2751,#2754,#213,.T.);
#3421=EDGE_CURVE('',#2755,#2756,#1687,.T.);
#3422=EDGE_CURVE('',#2756,#2752,#214,.T.);
#3423=EDGE_CURVE('',#2755,#2751,#215,.T.);
#3424=EDGE_CURVE('',#2757,#2758,#1688,.T.);
#3425=EDGE_CURVE('',#2758,#2756,#216,.T.);
#3426=EDGE_CURVE('',#2757,#2755,#217,.T.);
#3427=EDGE_CURVE('',#2759,#2760,#1689,.T.);
#3428=EDGE_CURVE('',#2760,#2758,#218,.T.);
#3429=EDGE_CURVE('',#2759,#2757,#219,.T.);
#3430=EDGE_CURVE('',#2761,#2762,#1690,.T.);
#3431=EDGE_CURVE('',#2762,#2760,#220,.T.);
#3432=EDGE_CURVE('',#2761,#2759,#221,.T.);
#3433=EDGE_CURVE('',#2763,#2764,#1691,.T.);
#3434=EDGE_CURVE('',#2764,#2762,#222,.T.);
#3435=EDGE_CURVE('',#2763,#2761,#223,.T.);
#3436=EDGE_CURVE('',#2765,#2766,#1692,.T.);
#3437=EDGE_CURVE('',#2766,#2764,#224,.T.);
#3438=EDGE_CURVE('',#2765,#2763,#225,.T.);
#3439=EDGE_CURVE('',#2767,#2768,#1693,.T.);
#3440=EDGE_CURVE('',#2769,#2767,#226,.T.);
#3441=EDGE_CURVE('',#2770,#2769,#2355,.T.);
#3442=EDGE_CURVE('',#2770,#2768,#227,.T.);
#3443=EDGE_CURVE('',#2771,#2772,#1694,.T.);
#3444=EDGE_CURVE('',#2772,#2773,#228,.T.);
#3445=EDGE_CURVE('',#2774,#2773,#2356,.T.);
#3446=EDGE_CURVE('',#2771,#2774,#229,.T.);
#3447=EDGE_CURVE('',#2775,#2776,#1695,.T.);
#3448=EDGE_CURVE('',#2776,#2772,#230,.T.);
#3449=EDGE_CURVE('',#2775,#2771,#231,.T.);
#3450=EDGE_CURVE('',#2777,#2778,#1696,.T.);
#3451=EDGE_CURVE('',#2778,#2776,#232,.T.);
#3452=EDGE_CURVE('',#2777,#2775,#233,.T.);
#3453=EDGE_CURVE('',#2779,#2780,#1697,.T.);
#3454=EDGE_CURVE('',#2780,#2778,#234,.T.);
#3455=EDGE_CURVE('',#2779,#2777,#235,.T.);
#3456=EDGE_CURVE('',#2781,#2782,#1698,.T.);
#3457=EDGE_CURVE('',#2782,#2780,#236,.T.);
#3458=EDGE_CURVE('',#2781,#2779,#237,.T.);
#3459=EDGE_CURVE('',#2783,#2784,#1699,.T.);
#3460=EDGE_CURVE('',#2784,#2782,#238,.T.);
#3461=EDGE_CURVE('',#2783,#2781,#239,.T.);
#3462=EDGE_CURVE('',#2785,#2786,#1700,.T.);
#3463=EDGE_CURVE('',#2786,#2784,#240,.T.);
#3464=EDGE_CURVE('',#2785,#2783,#241,.T.);
#3465=EDGE_CURVE('',#2787,#2788,#1701,.T.);
#3466=EDGE_CURVE('',#2789,#2787,#242,.T.);
#3467=EDGE_CURVE('',#2790,#2789,#2357,.T.);
#3468=EDGE_CURVE('',#2790,#2788,#243,.T.);
#3469=EDGE_CURVE('',#2791,#2792,#1702,.T.);
#3470=EDGE_CURVE('',#2792,#2793,#244,.T.);
#3471=EDGE_CURVE('',#2794,#2793,#2358,.T.);
#3472=EDGE_CURVE('',#2791,#2794,#245,.T.);
#3473=EDGE_CURVE('',#2795,#2796,#1703,.T.);
#3474=EDGE_CURVE('',#2796,#2792,#246,.T.);
#3475=EDGE_CURVE('',#2795,#2791,#247,.T.);
#3476=EDGE_CURVE('',#2797,#2798,#1704,.T.);
#3477=EDGE_CURVE('',#2798,#2796,#248,.T.);
#3478=EDGE_CURVE('',#2797,#2795,#249,.T.);
#3479=EDGE_CURVE('',#2799,#2800,#1705,.T.);
#3480=EDGE_CURVE('',#2800,#2798,#250,.T.);
#3481=EDGE_CURVE('',#2799,#2797,#251,.T.);
#3482=EDGE_CURVE('',#2801,#2802,#1706,.T.);
#3483=EDGE_CURVE('',#2802,#2800,#252,.T.);
#3484=EDGE_CURVE('',#2801,#2799,#253,.T.);
#3485=EDGE_CURVE('',#2803,#2804,#1707,.T.);
#3486=EDGE_CURVE('',#2804,#2802,#254,.T.);
#3487=EDGE_CURVE('',#2803,#2801,#255,.T.);
#3488=EDGE_CURVE('',#2805,#2806,#1708,.T.);
#3489=EDGE_CURVE('',#2806,#2804,#256,.T.);
#3490=EDGE_CURVE('',#2805,#2803,#257,.T.);
#3491=EDGE_CURVE('',#2807,#2808,#1709,.T.);
#3492=EDGE_CURVE('',#2809,#2807,#258,.T.);
#3493=EDGE_CURVE('',#2810,#2809,#2359,.T.);
#3494=EDGE_CURVE('',#2810,#2808,#259,.T.);
#3495=EDGE_CURVE('',#2811,#2812,#1710,.T.);
#3496=EDGE_CURVE('',#2812,#2813,#260,.T.);
#3497=EDGE_CURVE('',#2814,#2813,#2360,.T.);
#3498=EDGE_CURVE('',#2811,#2814,#261,.T.);
#3499=EDGE_CURVE('',#2815,#2816,#1711,.T.);
#3500=EDGE_CURVE('',#2816,#2812,#262,.T.);
#3501=EDGE_CURVE('',#2815,#2811,#263,.T.);
#3502=EDGE_CURVE('',#2817,#2818,#1712,.T.);
#3503=EDGE_CURVE('',#2818,#2816,#264,.T.);
#3504=EDGE_CURVE('',#2817,#2815,#265,.T.);
#3505=EDGE_CURVE('',#2819,#2820,#1713,.T.);
#3506=EDGE_CURVE('',#2820,#2818,#266,.T.);
#3507=EDGE_CURVE('',#2819,#2817,#267,.T.);
#3508=EDGE_CURVE('',#2821,#2822,#1714,.T.);
#3509=EDGE_CURVE('',#2822,#2820,#268,.T.);
#3510=EDGE_CURVE('',#2821,#2819,#269,.T.);
#3511=EDGE_CURVE('',#2823,#2824,#1715,.T.);
#3512=EDGE_CURVE('',#2824,#2822,#270,.T.);
#3513=EDGE_CURVE('',#2823,#2821,#271,.T.);
#3514=EDGE_CURVE('',#2825,#2826,#1716,.T.);
#3515=EDGE_CURVE('',#2826,#2824,#272,.T.);
#3516=EDGE_CURVE('',#2825,#2823,#273,.T.);
#3517=EDGE_CURVE('',#2827,#2828,#1717,.T.);
#3518=EDGE_CURVE('',#2829,#2827,#274,.T.);
#3519=EDGE_CURVE('',#2830,#2829,#2361,.T.);
#3520=EDGE_CURVE('',#2830,#2828,#275,.T.);
#3521=EDGE_CURVE('',#2831,#2831,#2362,.T.);
#3522=EDGE_CURVE('',#2831,#2832,#1718,.T.);
#3523=EDGE_CURVE('',#2832,#2832,#2363,.T.);
#3524=EDGE_CURVE('',#2833,#2833,#2364,.T.);
#3525=EDGE_CURVE('',#2833,#2834,#1719,.T.);
#3526=EDGE_CURVE('',#2834,#2834,#2365,.T.);
#3527=EDGE_CURVE('',#2835,#2836,#2366,.T.);
#3528=EDGE_CURVE('',#2836,#2837,#2367,.T.);
#3529=EDGE_CURVE('',#2837,#2838,#1720,.T.);
#3530=EDGE_CURVE('',#2838,#2839,#2368,.T.);
#3531=EDGE_CURVE('',#2839,#2835,#1721,.T.);
#3532=EDGE_CURVE('',#2840,#2841,#2369,.T.);
#3533=EDGE_CURVE('',#2841,#2842,#1722,.T.);
#3534=EDGE_CURVE('',#2842,#2843,#2370,.T.);
#3535=EDGE_CURVE('',#2843,#2840,#1723,.T.);
#3536=EDGE_CURVE('',#2844,#2845,#1724,.T.);
#3537=EDGE_CURVE('',#2845,#2846,#2371,.T.);
#3538=EDGE_CURVE('',#2846,#2847,#1725,.T.);
#3539=EDGE_CURVE('',#2847,#2844,#2372,.T.);
#3540=EDGE_CURVE('',#2848,#2848,#2373,.T.);
#3541=EDGE_CURVE('',#2828,#2826,#276,.T.);
#3542=EDGE_CURVE('',#2827,#2825,#277,.T.);
#3543=EDGE_CURVE('',#2813,#2674,#278,.T.);
#3544=EDGE_CURVE('',#2689,#2830,#279,.T.);
#3545=EDGE_CURVE('',#2685,#2687,#280,.T.);
#3546=EDGE_CURVE('',#2673,#2814,#281,.T.);
#3547=EDGE_CURVE('',#2688,#2686,#282,.T.);
#3548=EDGE_CURVE('',#2829,#2690,#283,.T.);
#3549=EDGE_CURVE('',#2849,#2849,#2374,.T.);
#3550=EDGE_CURVE('',#2850,#2850,#2375,.T.);
#3551=EDGE_CURVE('',#2693,#2754,#284,.T.);
#3552=EDGE_CURVE('',#2753,#2694,#285,.T.);
#3553=EDGE_CURVE('',#2713,#2774,#286,.T.);
#3554=EDGE_CURVE('',#2773,#2714,#287,.T.);
#3555=EDGE_CURVE('',#2733,#2794,#288,.T.);
#3556=EDGE_CURVE('',#2793,#2734,#289,.T.);
#3557=EDGE_CURVE('',#2808,#2806,#290,.T.);
#3558=EDGE_CURVE('',#2807,#2805,#291,.T.);
#3559=EDGE_CURVE('',#2749,#2810,#292,.T.);
#3560=EDGE_CURVE('',#2745,#2747,#293,.T.);
#3561=EDGE_CURVE('',#2748,#2746,#294,.T.);
#3562=EDGE_CURVE('',#2809,#2750,#295,.T.);
#3563=EDGE_CURVE('',#2788,#2786,#296,.T.);
#3564=EDGE_CURVE('',#2787,#2785,#297,.T.);
#3565=EDGE_CURVE('',#2729,#2790,#298,.T.);
#3566=EDGE_CURVE('',#2725,#2727,#299,.T.);
#3567=EDGE_CURVE('',#2728,#2726,#300,.T.);
#3568=EDGE_CURVE('',#2789,#2730,#301,.T.);
#3569=EDGE_CURVE('',#2768,#2766,#302,.T.);
#3570=EDGE_CURVE('',#2767,#2765,#303,.T.);
#3571=EDGE_CURVE('',#2709,#2770,#304,.T.);
#3572=EDGE_CURVE('',#2705,#2707,#305,.T.);
#3573=EDGE_CURVE('',#2708,#2706,#306,.T.);
#3574=EDGE_CURVE('',#2769,#2710,#307,.T.);
#3575=EDGE_CURVE('',#2851,#2851,#2376,.T.);
#3576=EDGE_CURVE('',#2851,#2852,#1726,.T.);
#3577=EDGE_CURVE('',#2852,#2852,#2377,.T.);
#3578=EDGE_CURVE('',#2853,#2853,#2378,.T.);
#3579=EDGE_CURVE('',#2853,#2854,#1727,.T.);
#3580=EDGE_CURVE('',#2854,#2854,#2379,.T.);
#3581=EDGE_CURVE('',#2855,#2855,#2380,.T.);
#3582=EDGE_CURVE('',#2855,#2856,#1728,.T.);
#3583=EDGE_CURVE('',#2856,#2856,#2381,.T.);
#3584=EDGE_CURVE('',#2857,#2857,#2382,.T.);
#3585=EDGE_CURVE('',#2857,#2858,#1729,.T.);
#3586=EDGE_CURVE('',#2858,#2858,#2383,.T.);
#3587=EDGE_CURVE('',#2859,#2859,#2384,.T.);
#3588=EDGE_CURVE('',#2860,#2860,#2385,.T.);
#3589=EDGE_CURVE('',#2859,#2861,#1730,.T.);
#3590=EDGE_CURVE('',#2861,#2861,#2386,.T.);
#3591=EDGE_CURVE('',#2862,#2862,#2387,.T.);
#3592=EDGE_CURVE('',#2850,#2860,#1731,.T.);
#3593=EDGE_CURVE('',#2835,#2863,#1732,.T.);
#3594=EDGE_CURVE('',#2864,#2839,#1733,.T.);
#3595=EDGE_CURVE('',#2864,#2863,#1734,.T.);
#3596=EDGE_CURVE('',#2865,#2844,#1735,.T.);
#3597=EDGE_CURVE('',#2865,#2866,#1736,.T.);
#3598=EDGE_CURVE('',#2845,#2866,#1737,.T.);
#3599=EDGE_CURVE('',#2840,#2867,#1738,.T.);
#3600=EDGE_CURVE('',#2868,#2843,#1739,.T.);
#3601=EDGE_CURVE('',#2868,#2867,#1740,.T.);
#3602=EDGE_CURVE('',#2869,#2837,#1741,.T.);
#3603=EDGE_CURVE('',#2869,#2870,#1742,.T.);
#3604=EDGE_CURVE('',#2838,#2870,#1743,.T.);
#3605=EDGE_CURVE('',#2847,#2871,#1744,.T.);
#3606=EDGE_CURVE('',#2872,#2871,#2388,.T.);
#3607=EDGE_CURVE('',#2872,#2841,#1745,.T.);
#3608=EDGE_CURVE('',#2869,#2867,#2389,.T.);
#3609=EDGE_CURVE('',#2836,#2862,#1746,.T.);
#3610=EDGE_CURVE('',#2865,#2863,#2390,.T.);
#3611=EDGE_CURVE('',#2873,#2871,#1747,.T.);
#3612=EDGE_CURVE('',#2866,#2873,#2391,.T.);
#3613=EDGE_CURVE('',#2870,#2864,#2392,.T.);
#3614=EDGE_CURVE('',#2874,#2868,#2393,.T.);
#3615=EDGE_CURVE('',#2872,#2874,#1748,.T.);
#3616=EDGE_CURVE('',#2875,#2875,#2394,.T.);
#3617=EDGE_CURVE('',#2874,#2842,#1749,.T.);
#3618=EDGE_CURVE('',#2848,#2875,#1750,.T.);
#3619=EDGE_CURVE('',#2846,#2873,#1751,.T.);
#3620=EDGE_CURVE('',#2876,#2876,#2395,.T.);
#3621=EDGE_CURVE('',#2876,#2849,#1752,.T.);
#3622=EDGE_CURVE('',#2877,#2877,#136,.T.);
#3623=EDGE_CURVE('',#2877,#2877,#2396,.T.);
#3624=EDGE_CURVE('',#2878,#2878,#2397,.T.);
#3625=EDGE_CURVE('',#2879,#2879,#2398,.T.);
#3626=EDGE_CURVE('',#2880,#2880,#2399,.T.);
#3627=EDGE_CURVE('',#2881,#2881,#2400,.T.);
#3628=EDGE_CURVE('',#2882,#2882,#2401,.T.);
#3629=EDGE_CURVE('',#2883,#2883,#2402,.T.);
#3630=EDGE_CURVE('',#2881,#2884,#1753,.T.);
#3631=EDGE_CURVE('',#2884,#2884,#2403,.T.);
#3632=EDGE_CURVE('',#2883,#2885,#1754,.T.);
#3633=EDGE_CURVE('',#2885,#2885,#2404,.T.);
#3634=EDGE_CURVE('',#2879,#2886,#1755,.T.);
#3635=EDGE_CURVE('',#2886,#2886,#2405,.T.);
#3636=EDGE_CURVE('',#2880,#2887,#1756,.T.);
#3637=EDGE_CURVE('',#2887,#2887,#2406,.T.);
#3638=EDGE_CURVE('',#2888,#2888,#2407,.T.);
#3639=EDGE_CURVE('',#2889,#2889,#2408,.T.);
#3640=EDGE_CURVE('',#2878,#2888,#1757,.T.);
#3641=EDGE_CURVE('',#2890,#2891,#1758,.T.);
#3642=EDGE_CURVE('',#2891,#2890,#2409,.T.);
#3643=EDGE_CURVE('',#2892,#2892,#2410,.T.);
#3644=EDGE_CURVE('',#2882,#2892,#1759,.T.);
#3645=EDGE_CURVE('',#2889,#2893,#1760,.T.);
#3646=EDGE_CURVE('',#2894,#2893,#308,.T.);
#3647=EDGE_CURVE('',#2893,#2894,#309,.T.);
#3648=EDGE_CURVE('',#2891,#2895,#1761,.T.);
#3649=EDGE_CURVE('',#2896,#2890,#1762,.T.);
#3650=EDGE_CURVE('',#2895,#2896,#310,.T.);
#3651=EDGE_CURVE('',#2897,#2896,#2411,.T.);
#3652=EDGE_CURVE('',#2897,#2898,#1763,.T.);
#3653=EDGE_CURVE('',#2898,#2898,#2412,.T.);
#3654=EDGE_CURVE('',#2895,#2897,#2413,.T.);
#3655=EDGE_CURVE('',#2899,#2899,#2414,.T.);
#3656=EDGE_CURVE('',#2899,#2900,#1764,.T.);
#3657=EDGE_CURVE('',#2900,#2900,#2415,.T.);
#3658=EDGE_CURVE('',#2901,#2901,#2416,.T.);
#3659=EDGE_CURVE('',#2901,#2902,#1765,.T.);
#3660=EDGE_CURVE('',#2902,#2902,#2417,.T.);
#3661=EDGE_CURVE('',#2903,#2903,#2418,.T.);
#3662=EDGE_CURVE('',#2903,#2904,#1766,.T.);
#3663=EDGE_CURVE('',#2904,#2904,#2419,.T.);
#3664=EDGE_CURVE('',#2905,#2905,#2420,.T.);
#3665=EDGE_CURVE('',#2905,#2906,#1767,.T.);
#3666=EDGE_CURVE('',#2906,#2906,#2421,.T.);
#3667=EDGE_CURVE('',#2907,#2907,#2422,.T.);
#3668=EDGE_CURVE('',#2907,#2908,#1768,.T.);
#3669=EDGE_CURVE('',#2908,#2908,#2423,.T.);
#3670=EDGE_CURVE('',#2909,#2909,#2424,.T.);
#3671=EDGE_CURVE('',#2909,#2910,#1769,.T.);
#3672=EDGE_CURVE('',#2910,#2910,#2425,.T.);
#3673=EDGE_CURVE('',#2911,#2911,#2426,.T.);
#3674=EDGE_CURVE('',#2912,#2912,#2427,.T.);
#3675=EDGE_CURVE('',#2913,#2913,#2428,.T.);
#3676=EDGE_CURVE('',#2913,#2914,#1770,.T.);
#3677=EDGE_CURVE('',#2914,#2914,#2429,.T.);
#3678=EDGE_CURVE('',#2915,#2915,#2430,.T.);
#3679=EDGE_CURVE('',#2915,#2911,#1771,.T.);
#3680=EDGE_CURVE('',#2916,#2916,#2431,.T.);
#3681=EDGE_CURVE('',#2916,#2912,#1772,.T.);
#3682=EDGE_CURVE('',#2917,#2918,#1773,.T.);
#3683=EDGE_CURVE('',#2919,#2917,#2432,.T.);
#3684=EDGE_CURVE('',#2919,#2920,#1774,.T.);
#3685=EDGE_CURVE('',#2918,#2920,#311,.T.);
#3686=EDGE_CURVE('',#2921,#2918,#312,.T.);
#3687=EDGE_CURVE('',#2922,#2921,#1775,.T.);
#3688=EDGE_CURVE('',#2917,#2922,#2433,.T.);
#3689=EDGE_CURVE('',#2917,#2918,#1776,.T.);
#3690=EDGE_CURVE('',#2920,#2923,#1777,.T.);
#3691=EDGE_CURVE('',#2919,#2924,#1778,.T.);
#3692=EDGE_CURVE('',#2924,#2923,#1779,.T.);
#3693=EDGE_CURVE('',#2923,#2925,#313,.T.);
#3694=EDGE_CURVE('',#2926,#2924,#2434,.T.);
#3695=EDGE_CURVE('',#2926,#2925,#1780,.T.);
#3696=EDGE_CURVE('',#2925,#2921,#1781,.T.);
#3697=EDGE_CURVE('',#2926,#2922,#1782,.T.);
#3698=EDGE_CURVE('',#2918,#2927,#2435,.T.);
#3699=EDGE_CURVE('',#2927,#2918,#2436,.T.);
#3700=EDGE_CURVE('',#2927,#2928,#1783,.T.);
#3701=EDGE_CURVE('',#2928,#2928,#2437,.T.);
#3702=EDGE_CURVE('',#2929,#2930,#1784,.T.);
#3703=EDGE_CURVE('',#2931,#2929,#1785,.T.);
#3704=EDGE_CURVE('',#2931,#2932,#1786,.T.);
#3705=EDGE_CURVE('',#2932,#2930,#1787,.T.);
#3706=EDGE_CURVE('',#2930,#2933,#314,.T.);
#3707=EDGE_CURVE('',#2934,#2932,#2438,.T.);
#3708=EDGE_CURVE('',#2934,#2933,#1788,.T.);
#3709=EDGE_CURVE('',#2933,#2935,#1789,.T.);
#3710=EDGE_CURVE('',#2934,#2936,#1790,.T.);
#3711=EDGE_CURVE('',#2936,#2935,#1791,.T.);
#3712=EDGE_CURVE('',#2935,#2929,#315,.T.);
#3713=EDGE_CURVE('',#2931,#2936,#2439,.T.);
#3714=EDGE_CURVE('',#2937,#2938,#1792,.T.);
#3715=EDGE_CURVE('',#2939,#2937,#1793,.T.);
#3716=EDGE_CURVE('',#2939,#2940,#1794,.T.);
#3717=EDGE_CURVE('',#2940,#2938,#1795,.T.);
#3718=EDGE_CURVE('',#2938,#2941,#316,.T.);
#3719=EDGE_CURVE('',#2942,#2940,#2440,.T.);
#3720=EDGE_CURVE('',#2942,#2941,#1796,.T.);
#3721=EDGE_CURVE('',#2941,#2943,#1797,.T.);
#3722=EDGE_CURVE('',#2942,#2944,#1798,.T.);
#3723=EDGE_CURVE('',#2944,#2943,#1799,.T.);
#3724=EDGE_CURVE('',#2943,#2937,#317,.T.);
#3725=EDGE_CURVE('',#2939,#2944,#2441,.T.);
#3726=EDGE_CURVE('',#2945,#2945,#2442,.T.);
#3727=EDGE_CURVE('',#2945,#2946,#1800,.T.);
#3728=EDGE_CURVE('',#2946,#2946,#2443,.T.);
#3729=EDGE_CURVE('',#2947,#2947,#2444,.T.);
#3730=EDGE_CURVE('',#2948,#2948,#2445,.T.);
#3731=EDGE_CURVE('',#2949,#2949,#2446,.T.);
#3732=EDGE_CURVE('',#2950,#2950,#2447,.T.);
#3733=EDGE_CURVE('',#2951,#2951,#2448,.T.);
#3734=EDGE_CURVE('',#2948,#2950,#1801,.T.);
#3735=EDGE_CURVE('',#2951,#2952,#1802,.T.);
#3736=EDGE_CURVE('',#2952,#2952,#2449,.T.);
#3737=EDGE_CURVE('',#2947,#2949,#1803,.T.);
#3738=EDGE_CURVE('',#2953,#2953,#2450,.T.);
#3739=EDGE_CURVE('',#2953,#2954,#1804,.T.);
#3740=EDGE_CURVE('',#2954,#2954,#2451,.T.);
#3741=EDGE_CURVE('',#2955,#2955,#2452,.T.);
#3742=EDGE_CURVE('',#2955,#2956,#1805,.T.);
#3743=EDGE_CURVE('',#2956,#2956,#2453,.T.);
#3744=EDGE_CURVE('',#2957,#2957,#2454,.T.);
#3745=EDGE_CURVE('',#2957,#2958,#1806,.T.);
#3746=EDGE_CURVE('',#2958,#2958,#2455,.T.);
#3747=EDGE_CURVE('',#2959,#2959,#2456,.T.);
#3748=EDGE_CURVE('',#2959,#2960,#1807,.T.);
#3749=EDGE_CURVE('',#2960,#2960,#2457,.T.);
#3750=EDGE_CURVE('',#2961,#2961,#2458,.T.);
#3751=EDGE_CURVE('',#2961,#2962,#1808,.T.);
#3752=EDGE_CURVE('',#2962,#2962,#2459,.T.);
#3753=EDGE_CURVE('',#2963,#2963,#2460,.T.);
#3754=EDGE_CURVE('',#2963,#2964,#1809,.T.);
#3755=EDGE_CURVE('',#2964,#2964,#2461,.T.);
#3756=EDGE_CURVE('',#2965,#2965,#2462,.T.);
#3757=EDGE_CURVE('',#2965,#2966,#1810,.T.);
#3758=EDGE_CURVE('',#2966,#2966,#2463,.T.);
#3759=EDGE_CURVE('',#2967,#2967,#2464,.T.);
#3760=EDGE_CURVE('',#2967,#2968,#1811,.T.);
#3761=EDGE_CURVE('',#2968,#2968,#2465,.T.);
#3762=EDGE_CURVE('',#2969,#2970,#1812,.T.);
#3763=EDGE_CURVE('',#2969,#2971,#1813,.T.);
#3764=EDGE_CURVE('',#2972,#2971,#1814,.T.);
#3765=EDGE_CURVE('',#2970,#2972,#1815,.T.);
#3766=EDGE_CURVE('',#2973,#2970,#2466,.T.);
#3767=EDGE_CURVE('',#2974,#2972,#2467,.T.);
#3768=EDGE_CURVE('',#2973,#2974,#1816,.T.);
#3769=EDGE_CURVE('',#2973,#2975,#1817,.T.);
#3770=EDGE_CURVE('',#2976,#2974,#1818,.T.);
#3771=EDGE_CURVE('',#2975,#2976,#1819,.T.);
#3772=EDGE_CURVE('',#2969,#2975,#2468,.T.);
#3773=EDGE_CURVE('',#2971,#2976,#2469,.T.);
#3774=EDGE_CURVE('',#2977,#2977,#2470,.T.);
#3775=EDGE_CURVE('',#2977,#2978,#1820,.T.);
#3776=EDGE_CURVE('',#2978,#2978,#2471,.T.);
#3777=EDGE_CURVE('',#2979,#2979,#2472,.T.);
#3778=EDGE_CURVE('',#2979,#2980,#1821,.T.);
#3779=EDGE_CURVE('',#2980,#2980,#2473,.T.);
#3780=EDGE_CURVE('',#2981,#2981,#2474,.T.);
#3781=EDGE_CURVE('',#2981,#2982,#1822,.T.);
#3782=EDGE_CURVE('',#2982,#2982,#2475,.T.);
#3783=EDGE_CURVE('',#2983,#2983,#2476,.T.);
#3784=EDGE_CURVE('',#2983,#2984,#1823,.T.);
#3785=EDGE_CURVE('',#2984,#2984,#2477,.T.);
#3786=EDGE_CURVE('',#2985,#2985,#2478,.T.);
#3787=EDGE_CURVE('',#2985,#2986,#1824,.T.);
#3788=EDGE_CURVE('',#2986,#2986,#2479,.T.);
#3789=EDGE_CURVE('',#2987,#2987,#2480,.T.);
#3790=EDGE_CURVE('',#2987,#2988,#1825,.T.);
#3791=EDGE_CURVE('',#2988,#2988,#2481,.T.);
#3792=EDGE_CURVE('',#2989,#2989,#2482,.T.);
#3793=EDGE_CURVE('',#2989,#2990,#1826,.T.);
#3794=EDGE_CURVE('',#2990,#2990,#2483,.T.);
#3795=EDGE_CURVE('',#2991,#2991,#2484,.T.);
#3796=EDGE_CURVE('',#2991,#2992,#1827,.T.);
#3797=EDGE_CURVE('',#2992,#2992,#2485,.T.);
#3798=EDGE_CURVE('',#2993,#2994,#1828,.T.);
#3799=EDGE_CURVE('',#2995,#2993,#1829,.T.);
#3800=EDGE_CURVE('',#2996,#2995,#1830,.T.);
#3801=EDGE_CURVE('',#2994,#2996,#1831,.T.);
#3802=EDGE_CURVE('',#2997,#2998,#1832,.T.);
#3803=EDGE_CURVE('',#2999,#2997,#1833,.T.);
#3804=EDGE_CURVE('',#3000,#2999,#1834,.T.);
#3805=EDGE_CURVE('',#2998,#3000,#1835,.T.);
#3806=EDGE_CURVE('',#2995,#3000,#2486,.T.);
#3807=EDGE_CURVE('',#2998,#2993,#2487,.T.);
#3808=EDGE_CURVE('',#2997,#2994,#2488,.T.);
#3809=EDGE_CURVE('',#2996,#2999,#2489,.T.);
#3810=EDGE_CURVE('',#3001,#3002,#1836,.T.);
#3811=EDGE_CURVE('',#3001,#3003,#318,.T.);
#3812=EDGE_CURVE('',#3003,#3004,#2490,.T.);
#3813=EDGE_CURVE('',#3004,#3005,#1837,.T.);
#3814=EDGE_CURVE('',#3005,#3005,#2491,.F.);
#3815=EDGE_CURVE('',#3004,#3006,#2492,.T.);
#3816=EDGE_CURVE('',#3006,#3002,#319,.T.);
#3817=EDGE_CURVE('',#3007,#3008,#1838,.T.);
#3818=EDGE_CURVE('',#3007,#3001,#320,.T.);
#3819=EDGE_CURVE('',#3002,#3008,#321,.T.);
#3820=EDGE_CURVE('',#3009,#3010,#1839,.T.);
#3821=EDGE_CURVE('',#3009,#3007,#322,.T.);
#3822=EDGE_CURVE('',#3008,#3010,#323,.T.);
#3823=EDGE_CURVE('',#3011,#3012,#1840,.T.);
#3824=EDGE_CURVE('',#3011,#3009,#324,.T.);
#3825=EDGE_CURVE('',#3010,#3012,#325,.T.);
#3826=EDGE_CURVE('',#3013,#3014,#1841,.T.);
#3827=EDGE_CURVE('',#3013,#3011,#326,.T.);
#3828=EDGE_CURVE('',#3012,#3014,#327,.T.);
#3829=EDGE_CURVE('',#3015,#3016,#1842,.T.);
#3830=EDGE_CURVE('',#3015,#3013,#328,.T.);
#3831=EDGE_CURVE('',#3014,#3016,#329,.T.);
#3832=EDGE_CURVE('',#3017,#3018,#1843,.T.);
#3833=EDGE_CURVE('',#3017,#3015,#330,.T.);
#3834=EDGE_CURVE('',#3016,#3018,#331,.T.);
#3835=EDGE_CURVE('',#3019,#3020,#1844,.T.);
#3836=EDGE_CURVE('',#3019,#3021,#332,.T.);
#3837=EDGE_CURVE('',#3021,#3022,#2493,.T.);
#3838=EDGE_CURVE('',#3020,#3022,#333,.T.);
#3839=EDGE_CURVE('',#3023,#3024,#1845,.T.);
#3840=EDGE_CURVE('',#3023,#3019,#334,.T.);
#3841=EDGE_CURVE('',#3024,#3020,#335,.T.);
#3842=EDGE_CURVE('',#3025,#3026,#1846,.T.);
#3843=EDGE_CURVE('',#3025,#3023,#336,.T.);
#3844=EDGE_CURVE('',#3026,#3024,#337,.T.);
#3845=EDGE_CURVE('',#3027,#3028,#1847,.T.);
#3846=EDGE_CURVE('',#3027,#3025,#338,.T.);
#3847=EDGE_CURVE('',#3028,#3026,#339,.T.);
#3848=EDGE_CURVE('',#3029,#3030,#1848,.T.);
#3849=EDGE_CURVE('',#3029,#3027,#340,.T.);
#3850=EDGE_CURVE('',#3030,#3028,#341,.T.);
#3851=EDGE_CURVE('',#3031,#3032,#1849,.T.);
#3852=EDGE_CURVE('',#3031,#3029,#342,.T.);
#3853=EDGE_CURVE('',#3032,#3030,#343,.T.);
#3854=EDGE_CURVE('',#3033,#3034,#1850,.T.);
#3855=EDGE_CURVE('',#3033,#3031,#344,.T.);
#3856=EDGE_CURVE('',#3034,#3032,#345,.T.);
#3857=EDGE_CURVE('',#3022,#3035,#346,.T.);
#3858=EDGE_CURVE('',#3036,#3021,#347,.T.);
#3859=EDGE_CURVE('',#3037,#3036,#2494,.T.);
#3860=EDGE_CURVE('',#3035,#3037,#348,.T.);
#3861=EDGE_CURVE('',#3035,#3038,#1851,.T.);
#3862=EDGE_CURVE('',#3038,#3038,#2495,.T.);
#3863=EDGE_CURVE('',#3039,#3033,#349,.T.);
#3864=EDGE_CURVE('',#3003,#3039,#350,.T.);
#3865=EDGE_CURVE('',#3036,#3017,#351,.T.);
#3866=EDGE_CURVE('',#3040,#3034,#352,.T.);
#3867=EDGE_CURVE('',#3039,#3040,#2496,.T.);
#3868=EDGE_CURVE('',#3018,#3037,#353,.T.);
#3869=EDGE_CURVE('',#3040,#3006,#354,.T.);
#3870=EDGE_CURVE('',#3041,#3042,#1852,.T.);
#3871=EDGE_CURVE('',#3041,#3043,#1853,.T.);
#3872=EDGE_CURVE('',#3043,#3044,#1854,.T.);
#3873=EDGE_CURVE('',#3042,#3044,#1855,.T.);
#3874=EDGE_CURVE('',#3045,#3041,#1856,.T.);
#3875=EDGE_CURVE('',#3045,#3046,#1857,.T.);
#3876=EDGE_CURVE('',#3046,#3043,#1858,.T.);
#3877=EDGE_CURVE('',#3047,#3045,#1859,.T.);
#3878=EDGE_CURVE('',#3047,#3048,#1860,.T.);
#3879=EDGE_CURVE('',#3048,#3046,#1861,.T.);
#3880=EDGE_CURVE('',#3049,#3047,#1862,.T.);
#3881=EDGE_CURVE('',#3049,#3050,#1863,.T.);
#3882=EDGE_CURVE('',#3050,#3048,#1864,.T.);
#3883=EDGE_CURVE('',#3051,#3049,#1865,.T.);
#3884=EDGE_CURVE('',#3051,#3052,#1866,.T.);
#3885=EDGE_CURVE('',#3052,#3050,#1867,.T.);
#3886=EDGE_CURVE('',#3042,#3051,#1868,.T.);
#3887=EDGE_CURVE('',#3044,#3052,#1869,.T.);
#3888=EDGE_CURVE('',#3053,#3053,#2497,.T.);
#3889=EDGE_CURVE('',#3053,#3054,#1870,.T.);
#3890=EDGE_CURVE('',#3054,#3054,#2498,.T.);
#3891=ORIENTED_EDGE('',*,*,#3055,.F.);
#3892=ORIENTED_EDGE('',*,*,#3056,.T.);
#3893=ORIENTED_EDGE('',*,*,#3057,.T.);
#3894=ORIENTED_EDGE('',*,*,#3056,.F.);
#3895=ORIENTED_EDGE('',*,*,#3058,.F.);
#3896=ORIENTED_EDGE('',*,*,#3059,.T.);
#3897=ORIENTED_EDGE('',*,*,#3060,.T.);
#3898=ORIENTED_EDGE('',*,*,#3059,.F.);
#3899=ORIENTED_EDGE('',*,*,#3060,.F.);
#3900=ORIENTED_EDGE('',*,*,#3057,.F.);
#3901=ORIENTED_EDGE('',*,*,#3055,.T.);
#3902=ORIENTED_EDGE('',*,*,#3061,.T.);
#3903=ORIENTED_EDGE('',*,*,#3062,.F.);
#3904=ORIENTED_EDGE('',*,*,#3063,.T.);
#3905=ORIENTED_EDGE('',*,*,#3064,.F.);
#3906=ORIENTED_EDGE('',*,*,#3063,.F.);
#3907=ORIENTED_EDGE('',*,*,#3065,.F.);
#3908=ORIENTED_EDGE('',*,*,#3066,.T.);
#3909=ORIENTED_EDGE('',*,*,#3067,.F.);
#3910=ORIENTED_EDGE('',*,*,#3066,.F.);
#3911=ORIENTED_EDGE('',*,*,#3068,.F.);
#3912=ORIENTED_EDGE('',*,*,#3069,.T.);
#3913=ORIENTED_EDGE('',*,*,#3070,.F.);
#3914=ORIENTED_EDGE('',*,*,#3069,.F.);
#3915=ORIENTED_EDGE('',*,*,#3071,.F.);
#3916=ORIENTED_EDGE('',*,*,#3072,.T.);
#3917=ORIENTED_EDGE('',*,*,#3073,.F.);
#3918=ORIENTED_EDGE('',*,*,#3072,.F.);
#3919=ORIENTED_EDGE('',*,*,#3074,.F.);
#3920=ORIENTED_EDGE('',*,*,#3075,.T.);
#3921=ORIENTED_EDGE('',*,*,#3076,.F.);
#3922=ORIENTED_EDGE('',*,*,#3077,.F.);
#3923=ORIENTED_EDGE('',*,*,#3078,.F.);
#3924=ORIENTED_EDGE('',*,*,#3077,.T.);
#3925=ORIENTED_EDGE('',*,*,#3079,.F.);
#3926=ORIENTED_EDGE('',*,*,#3080,.F.);
#3927=ORIENTED_EDGE('',*,*,#3081,.F.);
#3928=ORIENTED_EDGE('',*,*,#3080,.T.);
#3929=ORIENTED_EDGE('',*,*,#3082,.F.);
#3930=ORIENTED_EDGE('',*,*,#3083,.F.);
#3931=ORIENTED_EDGE('',*,*,#3084,.F.);
#3932=ORIENTED_EDGE('',*,*,#3083,.T.);
#3933=ORIENTED_EDGE('',*,*,#3085,.F.);
#3934=ORIENTED_EDGE('',*,*,#3075,.F.);
#3935=ORIENTED_EDGE('',*,*,#3085,.T.);
#3936=ORIENTED_EDGE('',*,*,#3082,.T.);
#3937=ORIENTED_EDGE('',*,*,#3079,.T.);
#3938=ORIENTED_EDGE('',*,*,#3076,.T.);
#3939=ORIENTED_EDGE('',*,*,#3086,.F.);
#3940=ORIENTED_EDGE('',*,*,#3087,.T.);
#3941=ORIENTED_EDGE('',*,*,#3088,.F.);
#3942=ORIENTED_EDGE('',*,*,#3089,.F.);
#3943=ORIENTED_EDGE('',*,*,#3090,.F.);
#3944=ORIENTED_EDGE('',*,*,#3089,.T.);
#3945=ORIENTED_EDGE('',*,*,#3091,.F.);
#3946=ORIENTED_EDGE('',*,*,#3092,.F.);
#3947=ORIENTED_EDGE('',*,*,#3093,.F.);
#3948=ORIENTED_EDGE('',*,*,#3092,.T.);
#3949=ORIENTED_EDGE('',*,*,#3094,.F.);
#3950=ORIENTED_EDGE('',*,*,#3095,.F.);
#3951=ORIENTED_EDGE('',*,*,#3096,.F.);
#3952=ORIENTED_EDGE('',*,*,#3095,.T.);
#3953=ORIENTED_EDGE('',*,*,#3097,.F.);
#3954=ORIENTED_EDGE('',*,*,#3087,.F.);
#3955=ORIENTED_EDGE('',*,*,#3097,.T.);
#3956=ORIENTED_EDGE('',*,*,#3094,.T.);
#3957=ORIENTED_EDGE('',*,*,#3091,.T.);
#3958=ORIENTED_EDGE('',*,*,#3088,.T.);
#3959=ORIENTED_EDGE('',*,*,#3098,.F.);
#3960=ORIENTED_EDGE('',*,*,#3099,.T.);
#3961=ORIENTED_EDGE('',*,*,#3100,.F.);
#3962=ORIENTED_EDGE('',*,*,#3101,.F.);
#3963=ORIENTED_EDGE('',*,*,#3102,.F.);
#3964=ORIENTED_EDGE('',*,*,#3101,.T.);
#3965=ORIENTED_EDGE('',*,*,#3103,.F.);
#3966=ORIENTED_EDGE('',*,*,#3104,.F.);
#3967=ORIENTED_EDGE('',*,*,#3105,.F.);
#3968=ORIENTED_EDGE('',*,*,#3104,.T.);
#3969=ORIENTED_EDGE('',*,*,#3106,.F.);
#3970=ORIENTED_EDGE('',*,*,#3107,.F.);
#3971=ORIENTED_EDGE('',*,*,#3108,.F.);
#3972=ORIENTED_EDGE('',*,*,#3107,.T.);
#3973=ORIENTED_EDGE('',*,*,#3109,.F.);
#3974=ORIENTED_EDGE('',*,*,#3099,.F.);
#3975=ORIENTED_EDGE('',*,*,#3109,.T.);
#3976=ORIENTED_EDGE('',*,*,#3106,.T.);
#3977=ORIENTED_EDGE('',*,*,#3103,.T.);
#3978=ORIENTED_EDGE('',*,*,#3100,.T.);
#3979=ORIENTED_EDGE('',*,*,#3110,.F.);
#3980=ORIENTED_EDGE('',*,*,#3111,.T.);
#3981=ORIENTED_EDGE('',*,*,#3112,.F.);
#3982=ORIENTED_EDGE('',*,*,#3113,.F.);
#3983=ORIENTED_EDGE('',*,*,#3114,.F.);
#3984=ORIENTED_EDGE('',*,*,#3113,.T.);
#3985=ORIENTED_EDGE('',*,*,#3115,.F.);
#3986=ORIENTED_EDGE('',*,*,#3116,.F.);
#3987=ORIENTED_EDGE('',*,*,#3117,.F.);
#3988=ORIENTED_EDGE('',*,*,#3116,.T.);
#3989=ORIENTED_EDGE('',*,*,#3118,.F.);
#3990=ORIENTED_EDGE('',*,*,#3119,.F.);
#3991=ORIENTED_EDGE('',*,*,#3120,.F.);
#3992=ORIENTED_EDGE('',*,*,#3119,.T.);
#3993=ORIENTED_EDGE('',*,*,#3121,.F.);
#3994=ORIENTED_EDGE('',*,*,#3111,.F.);
#3995=ORIENTED_EDGE('',*,*,#3121,.T.);
#3996=ORIENTED_EDGE('',*,*,#3118,.T.);
#3997=ORIENTED_EDGE('',*,*,#3115,.T.);
#3998=ORIENTED_EDGE('',*,*,#3112,.T.);
#3999=ORIENTED_EDGE('',*,*,#3122,.F.);
#4000=ORIENTED_EDGE('',*,*,#3123,.T.);
#4001=ORIENTED_EDGE('',*,*,#3124,.F.);
#4002=ORIENTED_EDGE('',*,*,#3125,.F.);
#4003=ORIENTED_EDGE('',*,*,#3126,.F.);
#4004=ORIENTED_EDGE('',*,*,#3125,.T.);
#4005=ORIENTED_EDGE('',*,*,#3127,.F.);
#4006=ORIENTED_EDGE('',*,*,#3128,.F.);
#4007=ORIENTED_EDGE('',*,*,#3129,.F.);
#4008=ORIENTED_EDGE('',*,*,#3128,.T.);
#4009=ORIENTED_EDGE('',*,*,#3130,.F.);
#4010=ORIENTED_EDGE('',*,*,#3131,.F.);
#4011=ORIENTED_EDGE('',*,*,#3132,.F.);
#4012=ORIENTED_EDGE('',*,*,#3131,.T.);
#4013=ORIENTED_EDGE('',*,*,#3133,.F.);
#4014=ORIENTED_EDGE('',*,*,#3123,.F.);
#4015=ORIENTED_EDGE('',*,*,#3133,.T.);
#4016=ORIENTED_EDGE('',*,*,#3130,.T.);
#4017=ORIENTED_EDGE('',*,*,#3127,.T.);
#4018=ORIENTED_EDGE('',*,*,#3124,.T.);
#4019=ORIENTED_EDGE('',*,*,#3134,.F.);
#4020=ORIENTED_EDGE('',*,*,#3135,.T.);
#4021=ORIENTED_EDGE('',*,*,#3136,.F.);
#4022=ORIENTED_EDGE('',*,*,#3137,.F.);
#4023=ORIENTED_EDGE('',*,*,#3138,.F.);
#4024=ORIENTED_EDGE('',*,*,#3137,.T.);
#4025=ORIENTED_EDGE('',*,*,#3139,.F.);
#4026=ORIENTED_EDGE('',*,*,#3140,.F.);
#4027=ORIENTED_EDGE('',*,*,#3141,.F.);
#4028=ORIENTED_EDGE('',*,*,#3140,.T.);
#4029=ORIENTED_EDGE('',*,*,#3142,.F.);
#4030=ORIENTED_EDGE('',*,*,#3143,.F.);
#4031=ORIENTED_EDGE('',*,*,#3144,.F.);
#4032=ORIENTED_EDGE('',*,*,#3143,.T.);
#4033=ORIENTED_EDGE('',*,*,#3145,.F.);
#4034=ORIENTED_EDGE('',*,*,#3135,.F.);
#4035=ORIENTED_EDGE('',*,*,#3145,.T.);
#4036=ORIENTED_EDGE('',*,*,#3142,.T.);
#4037=ORIENTED_EDGE('',*,*,#3139,.T.);
#4038=ORIENTED_EDGE('',*,*,#3136,.T.);
#4039=ORIENTED_EDGE('',*,*,#3146,.F.);
#4040=ORIENTED_EDGE('',*,*,#3147,.F.);
#4041=ORIENTED_EDGE('',*,*,#3148,.F.);
#4042=ORIENTED_EDGE('',*,*,#3149,.T.);
#4043=ORIENTED_EDGE('',*,*,#3150,.F.);
#4044=ORIENTED_EDGE('',*,*,#3151,.T.);
#4045=ORIENTED_EDGE('',*,*,#3152,.F.);
#4046=ORIENTED_EDGE('',*,*,#3153,.F.);
#4047=ORIENTED_EDGE('',*,*,#3154,.F.);
#4048=ORIENTED_EDGE('',*,*,#3155,.F.);
#4049=ORIENTED_EDGE('',*,*,#3156,.F.);
#4050=ORIENTED_EDGE('',*,*,#3157,.T.);
#4051=ORIENTED_EDGE('',*,*,#3158,.F.);
#4052=ORIENTED_EDGE('',*,*,#3159,.T.);
#4053=ORIENTED_EDGE('',*,*,#3160,.F.);
#4054=ORIENTED_EDGE('',*,*,#3161,.F.);
#4055=ORIENTED_EDGE('',*,*,#3162,.F.);
#4056=ORIENTED_EDGE('',*,*,#3157,.F.);
#4057=ORIENTED_EDGE('',*,*,#3163,.F.);
#4058=ORIENTED_EDGE('',*,*,#3159,.F.);
#4059=ORIENTED_EDGE('',*,*,#3164,.F.);
#4060=ORIENTED_EDGE('',*,*,#3165,.F.);
#4061=ORIENTED_EDGE('',*,*,#3166,.F.);
#4062=ORIENTED_EDGE('',*,*,#3167,.F.);
#4063=ORIENTED_EDGE('',*,*,#3168,.F.);
#4064=ORIENTED_EDGE('',*,*,#3149,.F.);
#4065=ORIENTED_EDGE('',*,*,#3169,.F.);
#4066=ORIENTED_EDGE('',*,*,#3151,.F.);
#4067=ORIENTED_EDGE('',*,*,#3170,.F.);
#4068=ORIENTED_EDGE('',*,*,#3158,.T.);
#4069=ORIENTED_EDGE('',*,*,#3171,.F.);
#4070=ORIENTED_EDGE('',*,*,#3172,.F.);
#4071=ORIENTED_EDGE('',*,*,#3164,.T.);
#4072=ORIENTED_EDGE('',*,*,#3150,.T.);
#4073=ORIENTED_EDGE('',*,*,#3173,.F.);
#4074=ORIENTED_EDGE('',*,*,#3154,.T.);
#4075=ORIENTED_EDGE('',*,*,#3162,.T.);
#4076=ORIENTED_EDGE('',*,*,#3146,.T.);
#4077=ORIENTED_EDGE('',*,*,#3168,.T.);
#4078=ORIENTED_EDGE('',*,*,#3174,.F.);
#4079=ORIENTED_EDGE('',*,*,#3175,.F.);
#4080=ORIENTED_EDGE('',*,*,#3176,.F.);
#4081=ORIENTED_EDGE('',*,*,#3177,.T.);
#4082=ORIENTED_EDGE('',*,*,#3170,.T.);
#4083=ORIENTED_EDGE('',*,*,#3177,.F.);
#4084=ORIENTED_EDGE('',*,*,#3175,.T.);
#4085=ORIENTED_EDGE('',*,*,#3178,.T.);
#4086=ORIENTED_EDGE('',*,*,#3179,.F.);
#4087=ORIENTED_EDGE('',*,*,#3180,.T.);
#4088=ORIENTED_EDGE('',*,*,#3171,.T.);
#4089=ORIENTED_EDGE('',*,*,#3161,.T.);
#4090=ORIENTED_EDGE('',*,*,#3181,.F.);
#4091=ORIENTED_EDGE('',*,*,#3155,.T.);
#4092=ORIENTED_EDGE('',*,*,#3173,.T.);
#4093=ORIENTED_EDGE('',*,*,#3153,.T.);
#4094=ORIENTED_EDGE('',*,*,#3182,.F.);
#4095=ORIENTED_EDGE('',*,*,#3147,.T.);
#4096=ORIENTED_EDGE('',*,*,#3176,.T.);
#4097=ORIENTED_EDGE('',*,*,#3134,.T.);
#4098=ORIENTED_EDGE('',*,*,#3138,.T.);
#4099=ORIENTED_EDGE('',*,*,#3141,.T.);
#4100=ORIENTED_EDGE('',*,*,#3144,.T.);
#4101=ORIENTED_EDGE('',*,*,#3122,.T.);
#4102=ORIENTED_EDGE('',*,*,#3126,.T.);
#4103=ORIENTED_EDGE('',*,*,#3129,.T.);
#4104=ORIENTED_EDGE('',*,*,#3132,.T.);
#4105=ORIENTED_EDGE('',*,*,#3110,.T.);
#4106=ORIENTED_EDGE('',*,*,#3114,.T.);
#4107=ORIENTED_EDGE('',*,*,#3117,.T.);
#4108=ORIENTED_EDGE('',*,*,#3120,.T.);
#4109=ORIENTED_EDGE('',*,*,#3098,.T.);
#4110=ORIENTED_EDGE('',*,*,#3102,.T.);
#4111=ORIENTED_EDGE('',*,*,#3105,.T.);
#4112=ORIENTED_EDGE('',*,*,#3108,.T.);
#4113=ORIENTED_EDGE('',*,*,#3086,.T.);
#4114=ORIENTED_EDGE('',*,*,#3090,.T.);
#4115=ORIENTED_EDGE('',*,*,#3093,.T.);
#4116=ORIENTED_EDGE('',*,*,#3096,.T.);
#4117=ORIENTED_EDGE('',*,*,#3074,.T.);
#4118=ORIENTED_EDGE('',*,*,#3078,.T.);
#4119=ORIENTED_EDGE('',*,*,#3081,.T.);
#4120=ORIENTED_EDGE('',*,*,#3084,.T.);
#4121=ORIENTED_EDGE('',*,*,#3174,.T.);
#4122=ORIENTED_EDGE('',*,*,#3167,.T.);
#4123=ORIENTED_EDGE('',*,*,#3183,.F.);
#4124=ORIENTED_EDGE('',*,*,#3178,.F.);
#4125=ORIENTED_EDGE('',*,*,#3172,.T.);
#4126=ORIENTED_EDGE('',*,*,#3180,.F.);
#4127=ORIENTED_EDGE('',*,*,#3184,.F.);
#4128=ORIENTED_EDGE('',*,*,#3165,.T.);
#4129=ORIENTED_EDGE('',*,*,#3061,.F.);
#4130=ORIENTED_EDGE('',*,*,#3185,.T.);
#4131=ORIENTED_EDGE('',*,*,#3186,.T.);
#4132=ORIENTED_EDGE('',*,*,#3185,.F.);
#4133=ORIENTED_EDGE('',*,*,#3152,.T.);
#4134=ORIENTED_EDGE('',*,*,#3169,.T.);
#4135=ORIENTED_EDGE('',*,*,#3148,.T.);
#4136=ORIENTED_EDGE('',*,*,#3182,.T.);
#4137=ORIENTED_EDGE('',*,*,#3160,.T.);
#4138=ORIENTED_EDGE('',*,*,#3163,.T.);
#4139=ORIENTED_EDGE('',*,*,#3156,.T.);
#4140=ORIENTED_EDGE('',*,*,#3181,.T.);
#4141=ORIENTED_EDGE('',*,*,#3183,.T.);
#4142=ORIENTED_EDGE('',*,*,#3166,.T.);
#4143=ORIENTED_EDGE('',*,*,#3184,.T.);
#4144=ORIENTED_EDGE('',*,*,#3179,.T.);
#4145=ORIENTED_EDGE('',*,*,#3187,.F.);
#4146=ORIENTED_EDGE('',*,*,#3188,.T.);
#4147=ORIENTED_EDGE('',*,*,#3189,.T.);
#4148=ORIENTED_EDGE('',*,*,#3188,.F.);
#4149=ORIENTED_EDGE('',*,*,#3187,.T.);
#4150=ORIENTED_EDGE('',*,*,#3062,.T.);
#4151=ORIENTED_EDGE('',*,*,#3065,.T.);
#4152=ORIENTED_EDGE('',*,*,#3068,.T.);
#4153=ORIENTED_EDGE('',*,*,#3071,.T.);
#4154=ORIENTED_EDGE('',*,*,#3058,.T.);
#4155=ORIENTED_EDGE('',*,*,#3189,.F.);
#4156=ORIENTED_EDGE('',*,*,#3186,.F.);
#4157=ORIENTED_EDGE('',*,*,#3073,.T.);
#4158=ORIENTED_EDGE('',*,*,#3070,.T.);
#4159=ORIENTED_EDGE('',*,*,#3067,.T.);
#4160=ORIENTED_EDGE('',*,*,#3064,.T.);
#4161=ORIENTED_EDGE('',*,*,#3190,.F.);
#4162=ORIENTED_EDGE('',*,*,#3191,.T.);
#4163=ORIENTED_EDGE('',*,*,#3192,.T.);
#4164=ORIENTED_EDGE('',*,*,#3191,.F.);
#4165=ORIENTED_EDGE('',*,*,#3193,.F.);
#4166=ORIENTED_EDGE('',*,*,#3194,.T.);
#4167=ORIENTED_EDGE('',*,*,#3195,.T.);
#4168=ORIENTED_EDGE('',*,*,#3194,.F.);
#4169=ORIENTED_EDGE('',*,*,#3195,.F.);
#4170=ORIENTED_EDGE('',*,*,#3192,.F.);
#4171=ORIENTED_EDGE('',*,*,#3190,.T.);
#4172=ORIENTED_EDGE('',*,*,#3196,.T.);
#4173=ORIENTED_EDGE('',*,*,#3197,.F.);
#4174=ORIENTED_EDGE('',*,*,#3198,.T.);
#4175=ORIENTED_EDGE('',*,*,#3199,.F.);
#4176=ORIENTED_EDGE('',*,*,#3198,.F.);
#4177=ORIENTED_EDGE('',*,*,#3200,.F.);
#4178=ORIENTED_EDGE('',*,*,#3201,.T.);
#4179=ORIENTED_EDGE('',*,*,#3202,.F.);
#4180=ORIENTED_EDGE('',*,*,#3201,.F.);
#4181=ORIENTED_EDGE('',*,*,#3203,.F.);
#4182=ORIENTED_EDGE('',*,*,#3204,.T.);
#4183=ORIENTED_EDGE('',*,*,#3205,.F.);
#4184=ORIENTED_EDGE('',*,*,#3204,.F.);
#4185=ORIENTED_EDGE('',*,*,#3206,.F.);
#4186=ORIENTED_EDGE('',*,*,#3207,.T.);
#4187=ORIENTED_EDGE('',*,*,#3208,.F.);
#4188=ORIENTED_EDGE('',*,*,#3207,.F.);
#4189=ORIENTED_EDGE('',*,*,#3196,.F.);
#4190=ORIENTED_EDGE('',*,*,#3209,.T.);
#4191=ORIENTED_EDGE('',*,*,#3210,.T.);
#4192=ORIENTED_EDGE('',*,*,#3209,.F.);
#4193=ORIENTED_EDGE('',*,*,#3211,.F.);
#4194=ORIENTED_EDGE('',*,*,#3212,.T.);
#4195=ORIENTED_EDGE('',*,*,#3213,.T.);
#4196=ORIENTED_EDGE('',*,*,#3212,.F.);
#4197=ORIENTED_EDGE('',*,*,#3211,.T.);
#4198=ORIENTED_EDGE('',*,*,#3197,.T.);
#4199=ORIENTED_EDGE('',*,*,#3200,.T.);
#4200=ORIENTED_EDGE('',*,*,#3203,.T.);
#4201=ORIENTED_EDGE('',*,*,#3206,.T.);
#4202=ORIENTED_EDGE('',*,*,#3193,.T.);
#4203=ORIENTED_EDGE('',*,*,#3213,.F.);
#4204=ORIENTED_EDGE('',*,*,#3210,.F.);
#4205=ORIENTED_EDGE('',*,*,#3208,.T.);
#4206=ORIENTED_EDGE('',*,*,#3205,.T.);
#4207=ORIENTED_EDGE('',*,*,#3202,.T.);
#4208=ORIENTED_EDGE('',*,*,#3199,.T.);
#4209=ORIENTED_EDGE('',*,*,#3214,.F.);
#4210=ORIENTED_EDGE('',*,*,#3215,.T.);
#4211=ORIENTED_EDGE('',*,*,#3216,.T.);
#4212=ORIENTED_EDGE('',*,*,#3217,.F.);
#4213=ORIENTED_EDGE('',*,*,#3218,.T.);
#4214=ORIENTED_EDGE('',*,*,#3219,.T.);
#4215=ORIENTED_EDGE('',*,*,#3220,.F.);
#4216=ORIENTED_EDGE('',*,*,#3216,.F.);
#4217=ORIENTED_EDGE('',*,*,#3221,.F.);
#4218=ORIENTED_EDGE('',*,*,#3222,.F.);
#4219=ORIENTED_EDGE('',*,*,#3219,.F.);
#4220=ORIENTED_EDGE('',*,*,#3223,.T.);
#4221=ORIENTED_EDGE('',*,*,#3224,.F.);
#4222=ORIENTED_EDGE('',*,*,#3223,.F.);
#4223=ORIENTED_EDGE('',*,*,#3218,.F.);
#4224=ORIENTED_EDGE('',*,*,#3215,.F.);
#4225=ORIENTED_EDGE('',*,*,#3225,.F.);
#4226=ORIENTED_EDGE('',*,*,#3226,.T.);
#4227=ORIENTED_EDGE('',*,*,#3227,.T.);
#4228=ORIENTED_EDGE('',*,*,#3228,.T.);
#4229=ORIENTED_EDGE('',*,*,#3229,.T.);
#4230=ORIENTED_EDGE('',*,*,#3230,.T.);
#4231=ORIENTED_EDGE('',*,*,#3231,.T.);
#4232=ORIENTED_EDGE('',*,*,#3232,.T.);
#4233=ORIENTED_EDGE('',*,*,#3233,.T.);
#4234=ORIENTED_EDGE('',*,*,#3234,.T.);
#4235=ORIENTED_EDGE('',*,*,#3235,.T.);
#4236=ORIENTED_EDGE('',*,*,#3236,.T.);
#4237=ORIENTED_EDGE('',*,*,#3237,.T.);
#4238=ORIENTED_EDGE('',*,*,#3238,.T.);
#4239=ORIENTED_EDGE('',*,*,#3239,.T.);
#4240=ORIENTED_EDGE('',*,*,#3240,.T.);
#4241=ORIENTED_EDGE('',*,*,#3241,.T.);
#4242=ORIENTED_EDGE('',*,*,#3242,.T.);
#4243=ORIENTED_EDGE('',*,*,#3243,.T.);
#4244=ORIENTED_EDGE('',*,*,#3244,.T.);
#4245=ORIENTED_EDGE('',*,*,#3245,.T.);
#4246=ORIENTED_EDGE('',*,*,#3246,.T.);
#4247=ORIENTED_EDGE('',*,*,#3247,.T.);
#4248=ORIENTED_EDGE('',*,*,#3248,.T.);
#4249=ORIENTED_EDGE('',*,*,#3249,.T.);
#4250=ORIENTED_EDGE('',*,*,#3217,.T.);
#4251=ORIENTED_EDGE('',*,*,#3220,.T.);
#4252=ORIENTED_EDGE('',*,*,#3222,.T.);
#4253=ORIENTED_EDGE('',*,*,#3250,.F.);
#4254=ORIENTED_EDGE('',*,*,#3251,.F.);
#4255=ORIENTED_EDGE('',*,*,#3252,.F.);
#4256=ORIENTED_EDGE('',*,*,#3253,.T.);
#4257=ORIENTED_EDGE('',*,*,#3226,.F.);
#4258=ORIENTED_EDGE('',*,*,#3254,.F.);
#4259=ORIENTED_EDGE('',*,*,#3255,.T.);
#4260=ORIENTED_EDGE('',*,*,#3254,.T.);
#4261=ORIENTED_EDGE('',*,*,#3229,.F.);
#4262=ORIENTED_EDGE('',*,*,#3256,.F.);
#4263=ORIENTED_EDGE('',*,*,#3257,.T.);
#4264=ORIENTED_EDGE('',*,*,#3256,.T.);
#4265=ORIENTED_EDGE('',*,*,#3228,.F.);
#4266=ORIENTED_EDGE('',*,*,#3258,.F.);
#4267=ORIENTED_EDGE('',*,*,#3259,.T.);
#4268=ORIENTED_EDGE('',*,*,#3258,.T.);
#4269=ORIENTED_EDGE('',*,*,#3227,.F.);
#4270=ORIENTED_EDGE('',*,*,#3253,.F.);
#4271=ORIENTED_EDGE('',*,*,#3259,.F.);
#4272=ORIENTED_EDGE('',*,*,#3252,.T.);
#4273=ORIENTED_EDGE('',*,*,#3255,.F.);
#4274=ORIENTED_EDGE('',*,*,#3257,.F.);
#4275=ORIENTED_EDGE('',*,*,#3260,.F.);
#4276=ORIENTED_EDGE('',*,*,#3261,.T.);
#4277=ORIENTED_EDGE('',*,*,#3230,.F.);
#4278=ORIENTED_EDGE('',*,*,#3262,.F.);
#4279=ORIENTED_EDGE('',*,*,#3263,.T.);
#4280=ORIENTED_EDGE('',*,*,#3262,.T.);
#4281=ORIENTED_EDGE('',*,*,#3233,.F.);
#4282=ORIENTED_EDGE('',*,*,#3264,.F.);
#4283=ORIENTED_EDGE('',*,*,#3265,.T.);
#4284=ORIENTED_EDGE('',*,*,#3264,.T.);
#4285=ORIENTED_EDGE('',*,*,#3232,.F.);
#4286=ORIENTED_EDGE('',*,*,#3266,.F.);
#4287=ORIENTED_EDGE('',*,*,#3267,.T.);
#4288=ORIENTED_EDGE('',*,*,#3266,.T.);
#4289=ORIENTED_EDGE('',*,*,#3231,.F.);
#4290=ORIENTED_EDGE('',*,*,#3261,.F.);
#4291=ORIENTED_EDGE('',*,*,#3267,.F.);
#4292=ORIENTED_EDGE('',*,*,#3260,.T.);
#4293=ORIENTED_EDGE('',*,*,#3263,.F.);
#4294=ORIENTED_EDGE('',*,*,#3265,.F.);
#4295=ORIENTED_EDGE('',*,*,#3268,.F.);
#4296=ORIENTED_EDGE('',*,*,#3269,.T.);
#4297=ORIENTED_EDGE('',*,*,#3234,.F.);
#4298=ORIENTED_EDGE('',*,*,#3270,.F.);
#4299=ORIENTED_EDGE('',*,*,#3271,.T.);
#4300=ORIENTED_EDGE('',*,*,#3270,.T.);
#4301=ORIENTED_EDGE('',*,*,#3237,.F.);
#4302=ORIENTED_EDGE('',*,*,#3272,.F.);
#4303=ORIENTED_EDGE('',*,*,#3273,.T.);
#4304=ORIENTED_EDGE('',*,*,#3272,.T.);
#4305=ORIENTED_EDGE('',*,*,#3236,.F.);
#4306=ORIENTED_EDGE('',*,*,#3274,.F.);
#4307=ORIENTED_EDGE('',*,*,#3275,.T.);
#4308=ORIENTED_EDGE('',*,*,#3274,.T.);
#4309=ORIENTED_EDGE('',*,*,#3235,.F.);
#4310=ORIENTED_EDGE('',*,*,#3269,.F.);
#4311=ORIENTED_EDGE('',*,*,#3275,.F.);
#4312=ORIENTED_EDGE('',*,*,#3268,.T.);
#4313=ORIENTED_EDGE('',*,*,#3271,.F.);
#4314=ORIENTED_EDGE('',*,*,#3273,.F.);
#4315=ORIENTED_EDGE('',*,*,#3276,.F.);
#4316=ORIENTED_EDGE('',*,*,#3277,.T.);
#4317=ORIENTED_EDGE('',*,*,#3238,.F.);
#4318=ORIENTED_EDGE('',*,*,#3278,.F.);
#4319=ORIENTED_EDGE('',*,*,#3279,.T.);
#4320=ORIENTED_EDGE('',*,*,#3278,.T.);
#4321=ORIENTED_EDGE('',*,*,#3241,.F.);
#4322=ORIENTED_EDGE('',*,*,#3280,.F.);
#4323=ORIENTED_EDGE('',*,*,#3281,.T.);
#4324=ORIENTED_EDGE('',*,*,#3280,.T.);
#4325=ORIENTED_EDGE('',*,*,#3240,.F.);
#4326=ORIENTED_EDGE('',*,*,#3282,.F.);
#4327=ORIENTED_EDGE('',*,*,#3283,.T.);
#4328=ORIENTED_EDGE('',*,*,#3282,.T.);
#4329=ORIENTED_EDGE('',*,*,#3239,.F.);
#4330=ORIENTED_EDGE('',*,*,#3277,.F.);
#4331=ORIENTED_EDGE('',*,*,#3283,.F.);
#4332=ORIENTED_EDGE('',*,*,#3276,.T.);
#4333=ORIENTED_EDGE('',*,*,#3279,.F.);
#4334=ORIENTED_EDGE('',*,*,#3281,.F.);
#4335=ORIENTED_EDGE('',*,*,#3284,.F.);
#4336=ORIENTED_EDGE('',*,*,#3285,.T.);
#4337=ORIENTED_EDGE('',*,*,#3242,.F.);
#4338=ORIENTED_EDGE('',*,*,#3286,.F.);
#4339=ORIENTED_EDGE('',*,*,#3287,.T.);
#4340=ORIENTED_EDGE('',*,*,#3286,.T.);
#4341=ORIENTED_EDGE('',*,*,#3245,.F.);
#4342=ORIENTED_EDGE('',*,*,#3288,.F.);
#4343=ORIENTED_EDGE('',*,*,#3289,.T.);
#4344=ORIENTED_EDGE('',*,*,#3288,.T.);
#4345=ORIENTED_EDGE('',*,*,#3244,.F.);
#4346=ORIENTED_EDGE('',*,*,#3290,.F.);
#4347=ORIENTED_EDGE('',*,*,#3291,.T.);
#4348=ORIENTED_EDGE('',*,*,#3290,.T.);
#4349=ORIENTED_EDGE('',*,*,#3243,.F.);
#4350=ORIENTED_EDGE('',*,*,#3285,.F.);
#4351=ORIENTED_EDGE('',*,*,#3291,.F.);
#4352=ORIENTED_EDGE('',*,*,#3284,.T.);
#4353=ORIENTED_EDGE('',*,*,#3287,.F.);
#4354=ORIENTED_EDGE('',*,*,#3289,.F.);
#4355=ORIENTED_EDGE('',*,*,#3292,.F.);
#4356=ORIENTED_EDGE('',*,*,#3293,.T.);
#4357=ORIENTED_EDGE('',*,*,#3246,.F.);
#4358=ORIENTED_EDGE('',*,*,#3294,.F.);
#4359=ORIENTED_EDGE('',*,*,#3295,.T.);
#4360=ORIENTED_EDGE('',*,*,#3294,.T.);
#4361=ORIENTED_EDGE('',*,*,#3249,.F.);
#4362=ORIENTED_EDGE('',*,*,#3296,.F.);
#4363=ORIENTED_EDGE('',*,*,#3297,.T.);
#4364=ORIENTED_EDGE('',*,*,#3296,.T.);
#4365=ORIENTED_EDGE('',*,*,#3248,.F.);
#4366=ORIENTED_EDGE('',*,*,#3298,.F.);
#4367=ORIENTED_EDGE('',*,*,#3299,.T.);
#4368=ORIENTED_EDGE('',*,*,#3298,.T.);
#4369=ORIENTED_EDGE('',*,*,#3247,.F.);
#4370=ORIENTED_EDGE('',*,*,#3293,.F.);
#4371=ORIENTED_EDGE('',*,*,#3299,.F.);
#4372=ORIENTED_EDGE('',*,*,#3292,.T.);
#4373=ORIENTED_EDGE('',*,*,#3295,.F.);
#4374=ORIENTED_EDGE('',*,*,#3297,.F.);
#4375=ORIENTED_EDGE('',*,*,#3300,.F.);
#4376=ORIENTED_EDGE('',*,*,#3301,.T.);
#4377=ORIENTED_EDGE('',*,*,#3302,.F.);
#4378=ORIENTED_EDGE('',*,*,#3301,.F.);
#4379=ORIENTED_EDGE('',*,*,#3300,.T.);
#4380=ORIENTED_EDGE('',*,*,#3303,.T.);
#4381=ORIENTED_EDGE('',*,*,#3303,.F.);
#4382=ORIENTED_EDGE('',*,*,#3304,.T.);
#4383=ORIENTED_EDGE('',*,*,#3250,.T.);
#4384=ORIENTED_EDGE('',*,*,#3221,.T.);
#4385=ORIENTED_EDGE('',*,*,#3224,.T.);
#4386=ORIENTED_EDGE('',*,*,#3214,.T.);
#4387=ORIENTED_EDGE('',*,*,#3251,.T.);
#4388=ORIENTED_EDGE('',*,*,#3304,.F.);
#4389=ORIENTED_EDGE('',*,*,#3305,.F.);
#4390=ORIENTED_EDGE('',*,*,#3306,.T.);
#4391=ORIENTED_EDGE('',*,*,#3225,.T.);
#4392=ORIENTED_EDGE('',*,*,#3306,.F.);
#4393=ORIENTED_EDGE('',*,*,#3305,.T.);
#4394=ORIENTED_EDGE('',*,*,#3302,.T.);
#4395=ORIENTED_EDGE('',*,*,#3307,.F.);
#4396=ORIENTED_EDGE('',*,*,#3308,.T.);
#4397=ORIENTED_EDGE('',*,*,#3309,.T.);
#4398=ORIENTED_EDGE('',*,*,#3308,.F.);
#4399=ORIENTED_EDGE('',*,*,#3310,.F.);
#4400=ORIENTED_EDGE('',*,*,#3311,.T.);
#4401=ORIENTED_EDGE('',*,*,#3312,.T.);
#4402=ORIENTED_EDGE('',*,*,#3311,.F.);
#4403=ORIENTED_EDGE('',*,*,#3310,.T.);
#4404=ORIENTED_EDGE('',*,*,#3307,.T.);
#4405=ORIENTED_EDGE('',*,*,#3312,.F.);
#4406=ORIENTED_EDGE('',*,*,#3309,.F.);
#4407=ORIENTED_EDGE('',*,*,#3313,.T.);
#4408=ORIENTED_EDGE('',*,*,#3314,.T.);
#4409=ORIENTED_EDGE('',*,*,#3315,.F.);
#4410=ORIENTED_EDGE('',*,*,#3316,.T.);
#4411=ORIENTED_EDGE('',*,*,#3317,.T.);
#4412=ORIENTED_EDGE('',*,*,#3318,.T.);
#4413=ORIENTED_EDGE('',*,*,#3313,.F.);
#4414=ORIENTED_EDGE('',*,*,#3319,.T.);
#4415=ORIENTED_EDGE('',*,*,#3320,.T.);
#4416=ORIENTED_EDGE('',*,*,#3321,.T.);
#4417=ORIENTED_EDGE('',*,*,#3317,.F.);
#4418=ORIENTED_EDGE('',*,*,#3322,.T.);
#4419=ORIENTED_EDGE('',*,*,#3323,.T.);
#4420=ORIENTED_EDGE('',*,*,#3324,.T.);
#4421=ORIENTED_EDGE('',*,*,#3320,.F.);
#4422=ORIENTED_EDGE('',*,*,#3325,.T.);
#4423=ORIENTED_EDGE('',*,*,#3326,.T.);
#4424=ORIENTED_EDGE('',*,*,#3327,.T.);
#4425=ORIENTED_EDGE('',*,*,#3323,.F.);
#4426=ORIENTED_EDGE('',*,*,#3328,.T.);
#4427=ORIENTED_EDGE('',*,*,#3329,.T.);
#4428=ORIENTED_EDGE('',*,*,#3330,.T.);
#4429=ORIENTED_EDGE('',*,*,#3326,.F.);
#4430=ORIENTED_EDGE('',*,*,#3331,.T.);
#4431=ORIENTED_EDGE('',*,*,#3332,.T.);
#4432=ORIENTED_EDGE('',*,*,#3333,.T.);
#4433=ORIENTED_EDGE('',*,*,#3329,.F.);
#4434=ORIENTED_EDGE('',*,*,#3334,.T.);
#4435=ORIENTED_EDGE('',*,*,#3335,.F.);
#4436=ORIENTED_EDGE('',*,*,#3336,.T.);
#4437=ORIENTED_EDGE('',*,*,#3337,.F.);
#4438=ORIENTED_EDGE('',*,*,#3338,.T.);
#4439=ORIENTED_EDGE('',*,*,#3339,.T.);
#4440=ORIENTED_EDGE('',*,*,#3340,.T.);
#4441=ORIENTED_EDGE('',*,*,#3341,.F.);
#4442=ORIENTED_EDGE('',*,*,#3342,.T.);
#4443=ORIENTED_EDGE('',*,*,#3343,.T.);
#4444=ORIENTED_EDGE('',*,*,#3344,.T.);
#4445=ORIENTED_EDGE('',*,*,#3339,.F.);
#4446=ORIENTED_EDGE('',*,*,#3345,.T.);
#4447=ORIENTED_EDGE('',*,*,#3346,.T.);
#4448=ORIENTED_EDGE('',*,*,#3347,.T.);
#4449=ORIENTED_EDGE('',*,*,#3343,.F.);
#4450=ORIENTED_EDGE('',*,*,#3348,.T.);
#4451=ORIENTED_EDGE('',*,*,#3349,.T.);
#4452=ORIENTED_EDGE('',*,*,#3350,.T.);
#4453=ORIENTED_EDGE('',*,*,#3346,.F.);
#4454=ORIENTED_EDGE('',*,*,#3351,.T.);
#4455=ORIENTED_EDGE('',*,*,#3352,.T.);
#4456=ORIENTED_EDGE('',*,*,#3353,.T.);
#4457=ORIENTED_EDGE('',*,*,#3349,.F.);
#4458=ORIENTED_EDGE('',*,*,#3354,.T.);
#4459=ORIENTED_EDGE('',*,*,#3355,.T.);
#4460=ORIENTED_EDGE('',*,*,#3356,.T.);
#4461=ORIENTED_EDGE('',*,*,#3352,.F.);
#4462=ORIENTED_EDGE('',*,*,#3357,.T.);
#4463=ORIENTED_EDGE('',*,*,#3358,.T.);
#4464=ORIENTED_EDGE('',*,*,#3359,.T.);
#4465=ORIENTED_EDGE('',*,*,#3355,.F.);
#4466=ORIENTED_EDGE('',*,*,#3360,.T.);
#4467=ORIENTED_EDGE('',*,*,#3361,.F.);
#4468=ORIENTED_EDGE('',*,*,#3362,.T.);
#4469=ORIENTED_EDGE('',*,*,#3363,.F.);
#4470=ORIENTED_EDGE('',*,*,#3364,.T.);
#4471=ORIENTED_EDGE('',*,*,#3365,.T.);
#4472=ORIENTED_EDGE('',*,*,#3366,.T.);
#4473=ORIENTED_EDGE('',*,*,#3367,.F.);
#4474=ORIENTED_EDGE('',*,*,#3368,.T.);
#4475=ORIENTED_EDGE('',*,*,#3369,.T.);
#4476=ORIENTED_EDGE('',*,*,#3370,.T.);
#4477=ORIENTED_EDGE('',*,*,#3365,.F.);
#4478=ORIENTED_EDGE('',*,*,#3371,.T.);
#4479=ORIENTED_EDGE('',*,*,#3372,.T.);
#4480=ORIENTED_EDGE('',*,*,#3373,.T.);
#4481=ORIENTED_EDGE('',*,*,#3369,.F.);
#4482=ORIENTED_EDGE('',*,*,#3374,.T.);
#4483=ORIENTED_EDGE('',*,*,#3375,.T.);
#4484=ORIENTED_EDGE('',*,*,#3376,.T.);
#4485=ORIENTED_EDGE('',*,*,#3372,.F.);
#4486=ORIENTED_EDGE('',*,*,#3377,.T.);
#4487=ORIENTED_EDGE('',*,*,#3378,.T.);
#4488=ORIENTED_EDGE('',*,*,#3379,.T.);
#4489=ORIENTED_EDGE('',*,*,#3375,.F.);
#4490=ORIENTED_EDGE('',*,*,#3380,.T.);
#4491=ORIENTED_EDGE('',*,*,#3381,.T.);
#4492=ORIENTED_EDGE('',*,*,#3382,.T.);
#4493=ORIENTED_EDGE('',*,*,#3378,.F.);
#4494=ORIENTED_EDGE('',*,*,#3383,.T.);
#4495=ORIENTED_EDGE('',*,*,#3384,.T.);
#4496=ORIENTED_EDGE('',*,*,#3385,.T.);
#4497=ORIENTED_EDGE('',*,*,#3381,.F.);
#4498=ORIENTED_EDGE('',*,*,#3386,.T.);
#4499=ORIENTED_EDGE('',*,*,#3387,.F.);
#4500=ORIENTED_EDGE('',*,*,#3388,.T.);
#4501=ORIENTED_EDGE('',*,*,#3389,.F.);
#4502=ORIENTED_EDGE('',*,*,#3390,.T.);
#4503=ORIENTED_EDGE('',*,*,#3391,.T.);
#4504=ORIENTED_EDGE('',*,*,#3392,.T.);
#4505=ORIENTED_EDGE('',*,*,#3393,.F.);
#4506=ORIENTED_EDGE('',*,*,#3394,.T.);
#4507=ORIENTED_EDGE('',*,*,#3395,.T.);
#4508=ORIENTED_EDGE('',*,*,#3396,.T.);
#4509=ORIENTED_EDGE('',*,*,#3391,.F.);
#4510=ORIENTED_EDGE('',*,*,#3397,.T.);
#4511=ORIENTED_EDGE('',*,*,#3398,.T.);
#4512=ORIENTED_EDGE('',*,*,#3399,.T.);
#4513=ORIENTED_EDGE('',*,*,#3395,.F.);
#4514=ORIENTED_EDGE('',*,*,#3400,.T.);
#4515=ORIENTED_EDGE('',*,*,#3401,.T.);
#4516=ORIENTED_EDGE('',*,*,#3402,.T.);
#4517=ORIENTED_EDGE('',*,*,#3398,.F.);
#4518=ORIENTED_EDGE('',*,*,#3403,.T.);
#4519=ORIENTED_EDGE('',*,*,#3404,.T.);
#4520=ORIENTED_EDGE('',*,*,#3405,.T.);
#4521=ORIENTED_EDGE('',*,*,#3401,.F.);
#4522=ORIENTED_EDGE('',*,*,#3406,.T.);
#4523=ORIENTED_EDGE('',*,*,#3407,.T.);
#4524=ORIENTED_EDGE('',*,*,#3408,.T.);
#4525=ORIENTED_EDGE('',*,*,#3404,.F.);
#4526=ORIENTED_EDGE('',*,*,#3409,.T.);
#4527=ORIENTED_EDGE('',*,*,#3410,.T.);
#4528=ORIENTED_EDGE('',*,*,#3411,.T.);
#4529=ORIENTED_EDGE('',*,*,#3407,.F.);
#4530=ORIENTED_EDGE('',*,*,#3412,.T.);
#4531=ORIENTED_EDGE('',*,*,#3413,.F.);
#4532=ORIENTED_EDGE('',*,*,#3414,.T.);
#4533=ORIENTED_EDGE('',*,*,#3415,.F.);
#4534=ORIENTED_EDGE('',*,*,#3416,.T.);
#4535=ORIENTED_EDGE('',*,*,#3417,.T.);
#4536=ORIENTED_EDGE('',*,*,#3418,.T.);
#4537=ORIENTED_EDGE('',*,*,#3419,.F.);
#4538=ORIENTED_EDGE('',*,*,#3420,.F.);
#4539=ORIENTED_EDGE('',*,*,#3421,.T.);
#4540=ORIENTED_EDGE('',*,*,#3422,.T.);
#4541=ORIENTED_EDGE('',*,*,#3417,.F.);
#4542=ORIENTED_EDGE('',*,*,#3423,.F.);
#4543=ORIENTED_EDGE('',*,*,#3424,.T.);
#4544=ORIENTED_EDGE('',*,*,#3425,.T.);
#4545=ORIENTED_EDGE('',*,*,#3421,.F.);
#4546=ORIENTED_EDGE('',*,*,#3426,.F.);
#4547=ORIENTED_EDGE('',*,*,#3427,.T.);
#4548=ORIENTED_EDGE('',*,*,#3428,.T.);
#4549=ORIENTED_EDGE('',*,*,#3424,.F.);
#4550=ORIENTED_EDGE('',*,*,#3429,.F.);
#4551=ORIENTED_EDGE('',*,*,#3430,.T.);
#4552=ORIENTED_EDGE('',*,*,#3431,.T.);
#4553=ORIENTED_EDGE('',*,*,#3427,.F.);
#4554=ORIENTED_EDGE('',*,*,#3432,.F.);
#4555=ORIENTED_EDGE('',*,*,#3433,.T.);
#4556=ORIENTED_EDGE('',*,*,#3434,.T.);
#4557=ORIENTED_EDGE('',*,*,#3430,.F.);
#4558=ORIENTED_EDGE('',*,*,#3435,.F.);
#4559=ORIENTED_EDGE('',*,*,#3436,.T.);
#4560=ORIENTED_EDGE('',*,*,#3437,.T.);
#4561=ORIENTED_EDGE('',*,*,#3433,.F.);
#4562=ORIENTED_EDGE('',*,*,#3438,.F.);
#4563=ORIENTED_EDGE('',*,*,#3439,.F.);
#4564=ORIENTED_EDGE('',*,*,#3440,.F.);
#4565=ORIENTED_EDGE('',*,*,#3441,.F.);
#4566=ORIENTED_EDGE('',*,*,#3442,.T.);
#4567=ORIENTED_EDGE('',*,*,#3443,.T.);
#4568=ORIENTED_EDGE('',*,*,#3444,.T.);
#4569=ORIENTED_EDGE('',*,*,#3445,.F.);
#4570=ORIENTED_EDGE('',*,*,#3446,.F.);
#4571=ORIENTED_EDGE('',*,*,#3447,.T.);
#4572=ORIENTED_EDGE('',*,*,#3448,.T.);
#4573=ORIENTED_EDGE('',*,*,#3443,.F.);
#4574=ORIENTED_EDGE('',*,*,#3449,.F.);
#4575=ORIENTED_EDGE('',*,*,#3450,.T.);
#4576=ORIENTED_EDGE('',*,*,#3451,.T.);
#4577=ORIENTED_EDGE('',*,*,#3447,.F.);
#4578=ORIENTED_EDGE('',*,*,#3452,.F.);
#4579=ORIENTED_EDGE('',*,*,#3453,.T.);
#4580=ORIENTED_EDGE('',*,*,#3454,.T.);
#4581=ORIENTED_EDGE('',*,*,#3450,.F.);
#4582=ORIENTED_EDGE('',*,*,#3455,.F.);
#4583=ORIENTED_EDGE('',*,*,#3456,.T.);
#4584=ORIENTED_EDGE('',*,*,#3457,.T.);
#4585=ORIENTED_EDGE('',*,*,#3453,.F.);
#4586=ORIENTED_EDGE('',*,*,#3458,.F.);
#4587=ORIENTED_EDGE('',*,*,#3459,.T.);
#4588=ORIENTED_EDGE('',*,*,#3460,.T.);
#4589=ORIENTED_EDGE('',*,*,#3456,.F.);
#4590=ORIENTED_EDGE('',*,*,#3461,.F.);
#4591=ORIENTED_EDGE('',*,*,#3462,.T.);
#4592=ORIENTED_EDGE('',*,*,#3463,.T.);
#4593=ORIENTED_EDGE('',*,*,#3459,.F.);
#4594=ORIENTED_EDGE('',*,*,#3464,.F.);
#4595=ORIENTED_EDGE('',*,*,#3465,.F.);
#4596=ORIENTED_EDGE('',*,*,#3466,.F.);
#4597=ORIENTED_EDGE('',*,*,#3467,.F.);
#4598=ORIENTED_EDGE('',*,*,#3468,.T.);
#4599=ORIENTED_EDGE('',*,*,#3469,.T.);
#4600=ORIENTED_EDGE('',*,*,#3470,.T.);
#4601=ORIENTED_EDGE('',*,*,#3471,.F.);
#4602=ORIENTED_EDGE('',*,*,#3472,.F.);
#4603=ORIENTED_EDGE('',*,*,#3473,.T.);
#4604=ORIENTED_EDGE('',*,*,#3474,.T.);
#4605=ORIENTED_EDGE('',*,*,#3469,.F.);
#4606=ORIENTED_EDGE('',*,*,#3475,.F.);
#4607=ORIENTED_EDGE('',*,*,#3476,.T.);
#4608=ORIENTED_EDGE('',*,*,#3477,.T.);
#4609=ORIENTED_EDGE('',*,*,#3473,.F.);
#4610=ORIENTED_EDGE('',*,*,#3478,.F.);
#4611=ORIENTED_EDGE('',*,*,#3479,.T.);
#4612=ORIENTED_EDGE('',*,*,#3480,.T.);
#4613=ORIENTED_EDGE('',*,*,#3476,.F.);
#4614=ORIENTED_EDGE('',*,*,#3481,.F.);
#4615=ORIENTED_EDGE('',*,*,#3482,.T.);
#4616=ORIENTED_EDGE('',*,*,#3483,.T.);
#4617=ORIENTED_EDGE('',*,*,#3479,.F.);
#4618=ORIENTED_EDGE('',*,*,#3484,.F.);
#4619=ORIENTED_EDGE('',*,*,#3485,.T.);
#4620=ORIENTED_EDGE('',*,*,#3486,.T.);
#4621=ORIENTED_EDGE('',*,*,#3482,.F.);
#4622=ORIENTED_EDGE('',*,*,#3487,.F.);
#4623=ORIENTED_EDGE('',*,*,#3488,.T.);
#4624=ORIENTED_EDGE('',*,*,#3489,.T.);
#4625=ORIENTED_EDGE('',*,*,#3485,.F.);
#4626=ORIENTED_EDGE('',*,*,#3490,.F.);
#4627=ORIENTED_EDGE('',*,*,#3491,.F.);
#4628=ORIENTED_EDGE('',*,*,#3492,.F.);
#4629=ORIENTED_EDGE('',*,*,#3493,.F.);
#4630=ORIENTED_EDGE('',*,*,#3494,.T.);
#4631=ORIENTED_EDGE('',*,*,#3495,.T.);
#4632=ORIENTED_EDGE('',*,*,#3496,.T.);
#4633=ORIENTED_EDGE('',*,*,#3497,.F.);
#4634=ORIENTED_EDGE('',*,*,#3498,.F.);
#4635=ORIENTED_EDGE('',*,*,#3499,.T.);
#4636=ORIENTED_EDGE('',*,*,#3500,.T.);
#4637=ORIENTED_EDGE('',*,*,#3495,.F.);
#4638=ORIENTED_EDGE('',*,*,#3501,.F.);
#4639=ORIENTED_EDGE('',*,*,#3502,.T.);
#4640=ORIENTED_EDGE('',*,*,#3503,.T.);
#4641=ORIENTED_EDGE('',*,*,#3499,.F.);
#4642=ORIENTED_EDGE('',*,*,#3504,.F.);
#4643=ORIENTED_EDGE('',*,*,#3505,.T.);
#4644=ORIENTED_EDGE('',*,*,#3506,.T.);
#4645=ORIENTED_EDGE('',*,*,#3502,.F.);
#4646=ORIENTED_EDGE('',*,*,#3507,.F.);
#4647=ORIENTED_EDGE('',*,*,#3508,.T.);
#4648=ORIENTED_EDGE('',*,*,#3509,.T.);
#4649=ORIENTED_EDGE('',*,*,#3505,.F.);
#4650=ORIENTED_EDGE('',*,*,#3510,.F.);
#4651=ORIENTED_EDGE('',*,*,#3511,.T.);
#4652=ORIENTED_EDGE('',*,*,#3512,.T.);
#4653=ORIENTED_EDGE('',*,*,#3508,.F.);
#4654=ORIENTED_EDGE('',*,*,#3513,.F.);
#4655=ORIENTED_EDGE('',*,*,#3514,.T.);
#4656=ORIENTED_EDGE('',*,*,#3515,.T.);
#4657=ORIENTED_EDGE('',*,*,#3511,.F.);
#4658=ORIENTED_EDGE('',*,*,#3516,.F.);
#4659=ORIENTED_EDGE('',*,*,#3517,.F.);
#4660=ORIENTED_EDGE('',*,*,#3518,.F.);
#4661=ORIENTED_EDGE('',*,*,#3519,.F.);
#4662=ORIENTED_EDGE('',*,*,#3520,.T.);
#4663=ORIENTED_EDGE('',*,*,#3521,.F.);
#4664=ORIENTED_EDGE('',*,*,#3522,.T.);
#4665=ORIENTED_EDGE('',*,*,#3523,.T.);
#4666=ORIENTED_EDGE('',*,*,#3522,.F.);
#4667=ORIENTED_EDGE('',*,*,#3524,.F.);
#4668=ORIENTED_EDGE('',*,*,#3525,.T.);
#4669=ORIENTED_EDGE('',*,*,#3526,.T.);
#4670=ORIENTED_EDGE('',*,*,#3525,.F.);
#4671=ORIENTED_EDGE('',*,*,#3526,.F.);
#4672=ORIENTED_EDGE('',*,*,#3523,.F.);
#4673=ORIENTED_EDGE('',*,*,#3521,.T.);
#4674=ORIENTED_EDGE('',*,*,#3527,.T.);
#4675=ORIENTED_EDGE('',*,*,#3528,.T.);
#4676=ORIENTED_EDGE('',*,*,#3529,.T.);
#4677=ORIENTED_EDGE('',*,*,#3530,.T.);
#4678=ORIENTED_EDGE('',*,*,#3531,.T.);
#4679=ORIENTED_EDGE('',*,*,#3532,.T.);
#4680=ORIENTED_EDGE('',*,*,#3533,.T.);
#4681=ORIENTED_EDGE('',*,*,#3534,.T.);
#4682=ORIENTED_EDGE('',*,*,#3535,.T.);
#4683=ORIENTED_EDGE('',*,*,#3536,.T.);
#4684=ORIENTED_EDGE('',*,*,#3537,.T.);
#4685=ORIENTED_EDGE('',*,*,#3538,.T.);
#4686=ORIENTED_EDGE('',*,*,#3539,.T.);
#4687=ORIENTED_EDGE('',*,*,#3540,.T.);
#4688=ORIENTED_EDGE('',*,*,#3517,.T.);
#4689=ORIENTED_EDGE('',*,*,#3541,.T.);
#4690=ORIENTED_EDGE('',*,*,#3514,.F.);
#4691=ORIENTED_EDGE('',*,*,#3542,.F.);
#4692=ORIENTED_EDGE('',*,*,#3543,.F.);
#4693=ORIENTED_EDGE('',*,*,#3496,.F.);
#4694=ORIENTED_EDGE('',*,*,#3500,.F.);
#4695=ORIENTED_EDGE('',*,*,#3503,.F.);
#4696=ORIENTED_EDGE('',*,*,#3506,.F.);
#4697=ORIENTED_EDGE('',*,*,#3509,.F.);
#4698=ORIENTED_EDGE('',*,*,#3512,.F.);
#4699=ORIENTED_EDGE('',*,*,#3515,.F.);
#4700=ORIENTED_EDGE('',*,*,#3541,.F.);
#4701=ORIENTED_EDGE('',*,*,#3520,.F.);
#4702=ORIENTED_EDGE('',*,*,#3544,.F.);
#4703=ORIENTED_EDGE('',*,*,#3336,.F.);
#4704=ORIENTED_EDGE('',*,*,#3545,.F.);
#4705=ORIENTED_EDGE('',*,*,#3334,.F.);
#4706=ORIENTED_EDGE('',*,*,#3331,.F.);
#4707=ORIENTED_EDGE('',*,*,#3328,.F.);
#4708=ORIENTED_EDGE('',*,*,#3325,.F.);
#4709=ORIENTED_EDGE('',*,*,#3322,.F.);
#4710=ORIENTED_EDGE('',*,*,#3319,.F.);
#4711=ORIENTED_EDGE('',*,*,#3316,.F.);
#4712=ORIENTED_EDGE('',*,*,#3546,.F.);
#4713=ORIENTED_EDGE('',*,*,#3314,.F.);
#4714=ORIENTED_EDGE('',*,*,#3318,.F.);
#4715=ORIENTED_EDGE('',*,*,#3321,.F.);
#4716=ORIENTED_EDGE('',*,*,#3324,.F.);
#4717=ORIENTED_EDGE('',*,*,#3327,.F.);
#4718=ORIENTED_EDGE('',*,*,#3330,.F.);
#4719=ORIENTED_EDGE('',*,*,#3333,.F.);
#4720=ORIENTED_EDGE('',*,*,#3547,.F.);
#4721=ORIENTED_EDGE('',*,*,#3338,.F.);
#4722=ORIENTED_EDGE('',*,*,#3548,.F.);
#4723=ORIENTED_EDGE('',*,*,#3518,.T.);
#4724=ORIENTED_EDGE('',*,*,#3542,.T.);
#4725=ORIENTED_EDGE('',*,*,#3516,.T.);
#4726=ORIENTED_EDGE('',*,*,#3513,.T.);
#4727=ORIENTED_EDGE('',*,*,#3510,.T.);
#4728=ORIENTED_EDGE('',*,*,#3507,.T.);
#4729=ORIENTED_EDGE('',*,*,#3504,.T.);
#4730=ORIENTED_EDGE('',*,*,#3501,.T.);
#4731=ORIENTED_EDGE('',*,*,#3498,.T.);
#4732=ORIENTED_EDGE('',*,*,#3549,.F.);
#4733=ORIENTED_EDGE('',*,*,#3550,.T.);
#4734=ORIENTED_EDGE('',*,*,#3546,.T.);
#4735=ORIENTED_EDGE('',*,*,#3497,.T.);
#4736=ORIENTED_EDGE('',*,*,#3543,.T.);
#4737=ORIENTED_EDGE('',*,*,#3315,.T.);
#4738=ORIENTED_EDGE('',*,*,#3551,.T.);
#4739=ORIENTED_EDGE('',*,*,#3419,.T.);
#4740=ORIENTED_EDGE('',*,*,#3552,.T.);
#4741=ORIENTED_EDGE('',*,*,#3341,.T.);
#4742=ORIENTED_EDGE('',*,*,#3553,.T.);
#4743=ORIENTED_EDGE('',*,*,#3445,.T.);
#4744=ORIENTED_EDGE('',*,*,#3554,.T.);
#4745=ORIENTED_EDGE('',*,*,#3367,.T.);
#4746=ORIENTED_EDGE('',*,*,#3555,.T.);
#4747=ORIENTED_EDGE('',*,*,#3471,.T.);
#4748=ORIENTED_EDGE('',*,*,#3556,.T.);
#4749=ORIENTED_EDGE('',*,*,#3393,.T.);
#4750=ORIENTED_EDGE('',*,*,#3491,.T.);
#4751=ORIENTED_EDGE('',*,*,#3557,.T.);
#4752=ORIENTED_EDGE('',*,*,#3488,.F.);
#4753=ORIENTED_EDGE('',*,*,#3558,.F.);
#4754=ORIENTED_EDGE('',*,*,#3556,.F.);
#4755=ORIENTED_EDGE('',*,*,#3470,.F.);
#4756=ORIENTED_EDGE('',*,*,#3474,.F.);
#4757=ORIENTED_EDGE('',*,*,#3477,.F.);
#4758=ORIENTED_EDGE('',*,*,#3480,.F.);
#4759=ORIENTED_EDGE('',*,*,#3483,.F.);
#4760=ORIENTED_EDGE('',*,*,#3486,.F.);
#4761=ORIENTED_EDGE('',*,*,#3489,.F.);
#4762=ORIENTED_EDGE('',*,*,#3557,.F.);
#4763=ORIENTED_EDGE('',*,*,#3494,.F.);
#4764=ORIENTED_EDGE('',*,*,#3559,.F.);
#4765=ORIENTED_EDGE('',*,*,#3414,.F.);
#4766=ORIENTED_EDGE('',*,*,#3560,.F.);
#4767=ORIENTED_EDGE('',*,*,#3412,.F.);
#4768=ORIENTED_EDGE('',*,*,#3409,.F.);
#4769=ORIENTED_EDGE('',*,*,#3406,.F.);
#4770=ORIENTED_EDGE('',*,*,#3403,.F.);
#4771=ORIENTED_EDGE('',*,*,#3400,.F.);
#4772=ORIENTED_EDGE('',*,*,#3397,.F.);
#4773=ORIENTED_EDGE('',*,*,#3394,.F.);
#4774=ORIENTED_EDGE('',*,*,#3555,.F.);
#4775=ORIENTED_EDGE('',*,*,#3392,.F.);
#4776=ORIENTED_EDGE('',*,*,#3396,.F.);
#4777=ORIENTED_EDGE('',*,*,#3399,.F.);
#4778=ORIENTED_EDGE('',*,*,#3402,.F.);
#4779=ORIENTED_EDGE('',*,*,#3405,.F.);
#4780=ORIENTED_EDGE('',*,*,#3408,.F.);
#4781=ORIENTED_EDGE('',*,*,#3411,.F.);
#4782=ORIENTED_EDGE('',*,*,#3561,.F.);
#4783=ORIENTED_EDGE('',*,*,#3416,.F.);
#4784=ORIENTED_EDGE('',*,*,#3562,.F.);
#4785=ORIENTED_EDGE('',*,*,#3492,.T.);
#4786=ORIENTED_EDGE('',*,*,#3558,.T.);
#4787=ORIENTED_EDGE('',*,*,#3490,.T.);
#4788=ORIENTED_EDGE('',*,*,#3487,.T.);
#4789=ORIENTED_EDGE('',*,*,#3484,.T.);
#4790=ORIENTED_EDGE('',*,*,#3481,.T.);
#4791=ORIENTED_EDGE('',*,*,#3478,.T.);
#4792=ORIENTED_EDGE('',*,*,#3475,.T.);
#4793=ORIENTED_EDGE('',*,*,#3472,.T.);
#4794=ORIENTED_EDGE('',*,*,#3465,.T.);
#4795=ORIENTED_EDGE('',*,*,#3563,.T.);
#4796=ORIENTED_EDGE('',*,*,#3462,.F.);
#4797=ORIENTED_EDGE('',*,*,#3564,.F.);
#4798=ORIENTED_EDGE('',*,*,#3554,.F.);
#4799=ORIENTED_EDGE('',*,*,#3444,.F.);
#4800=ORIENTED_EDGE('',*,*,#3448,.F.);
#4801=ORIENTED_EDGE('',*,*,#3451,.F.);
#4802=ORIENTED_EDGE('',*,*,#3454,.F.);
#4803=ORIENTED_EDGE('',*,*,#3457,.F.);
#4804=ORIENTED_EDGE('',*,*,#3460,.F.);
#4805=ORIENTED_EDGE('',*,*,#3463,.F.);
#4806=ORIENTED_EDGE('',*,*,#3563,.F.);
#4807=ORIENTED_EDGE('',*,*,#3468,.F.);
#4808=ORIENTED_EDGE('',*,*,#3565,.F.);
#4809=ORIENTED_EDGE('',*,*,#3388,.F.);
#4810=ORIENTED_EDGE('',*,*,#3566,.F.);
#4811=ORIENTED_EDGE('',*,*,#3386,.F.);
#4812=ORIENTED_EDGE('',*,*,#3383,.F.);
#4813=ORIENTED_EDGE('',*,*,#3380,.F.);
#4814=ORIENTED_EDGE('',*,*,#3377,.F.);
#4815=ORIENTED_EDGE('',*,*,#3374,.F.);
#4816=ORIENTED_EDGE('',*,*,#3371,.F.);
#4817=ORIENTED_EDGE('',*,*,#3368,.F.);
#4818=ORIENTED_EDGE('',*,*,#3553,.F.);
#4819=ORIENTED_EDGE('',*,*,#3366,.F.);
#4820=ORIENTED_EDGE('',*,*,#3370,.F.);
#4821=ORIENTED_EDGE('',*,*,#3373,.F.);
#4822=ORIENTED_EDGE('',*,*,#3376,.F.);
#4823=ORIENTED_EDGE('',*,*,#3379,.F.);
#4824=ORIENTED_EDGE('',*,*,#3382,.F.);
#4825=ORIENTED_EDGE('',*,*,#3385,.F.);
#4826=ORIENTED_EDGE('',*,*,#3567,.F.);
#4827=ORIENTED_EDGE('',*,*,#3390,.F.);
#4828=ORIENTED_EDGE('',*,*,#3568,.F.);
#4829=ORIENTED_EDGE('',*,*,#3466,.T.);
#4830=ORIENTED_EDGE('',*,*,#3564,.T.);
#4831=ORIENTED_EDGE('',*,*,#3464,.T.);
#4832=ORIENTED_EDGE('',*,*,#3461,.T.);
#4833=ORIENTED_EDGE('',*,*,#3458,.T.);
#4834=ORIENTED_EDGE('',*,*,#3455,.T.);
#4835=ORIENTED_EDGE('',*,*,#3452,.T.);
#4836=ORIENTED_EDGE('',*,*,#3449,.T.);
#4837=ORIENTED_EDGE('',*,*,#3446,.T.);
#4838=ORIENTED_EDGE('',*,*,#3439,.T.);
#4839=ORIENTED_EDGE('',*,*,#3569,.T.);
#4840=ORIENTED_EDGE('',*,*,#3436,.F.);
#4841=ORIENTED_EDGE('',*,*,#3570,.F.);
#4842=ORIENTED_EDGE('',*,*,#3552,.F.);
#4843=ORIENTED_EDGE('',*,*,#3418,.F.);
#4844=ORIENTED_EDGE('',*,*,#3422,.F.);
#4845=ORIENTED_EDGE('',*,*,#3425,.F.);
#4846=ORIENTED_EDGE('',*,*,#3428,.F.);
#4847=ORIENTED_EDGE('',*,*,#3431,.F.);
#4848=ORIENTED_EDGE('',*,*,#3434,.F.);
#4849=ORIENTED_EDGE('',*,*,#3437,.F.);
#4850=ORIENTED_EDGE('',*,*,#3569,.F.);
#4851=ORIENTED_EDGE('',*,*,#3442,.F.);
#4852=ORIENTED_EDGE('',*,*,#3571,.F.);
#4853=ORIENTED_EDGE('',*,*,#3362,.F.);
#4854=ORIENTED_EDGE('',*,*,#3572,.F.);
#4855=ORIENTED_EDGE('',*,*,#3360,.F.);
#4856=ORIENTED_EDGE('',*,*,#3357,.F.);
#4857=ORIENTED_EDGE('',*,*,#3354,.F.);
#4858=ORIENTED_EDGE('',*,*,#3351,.F.);
#4859=ORIENTED_EDGE('',*,*,#3348,.F.);
#4860=ORIENTED_EDGE('',*,*,#3345,.F.);
#4861=ORIENTED_EDGE('',*,*,#3342,.F.);
#4862=ORIENTED_EDGE('',*,*,#3551,.F.);
#4863=ORIENTED_EDGE('',*,*,#3340,.F.);
#4864=ORIENTED_EDGE('',*,*,#3344,.F.);
#4865=ORIENTED_EDGE('',*,*,#3347,.F.);
#4866=ORIENTED_EDGE('',*,*,#3350,.F.);
#4867=ORIENTED_EDGE('',*,*,#3353,.F.);
#4868=ORIENTED_EDGE('',*,*,#3356,.F.);
#4869=ORIENTED_EDGE('',*,*,#3359,.F.);
#4870=ORIENTED_EDGE('',*,*,#3573,.F.);
#4871=ORIENTED_EDGE('',*,*,#3364,.F.);
#4872=ORIENTED_EDGE('',*,*,#3574,.F.);
#4873=ORIENTED_EDGE('',*,*,#3440,.T.);
#4874=ORIENTED_EDGE('',*,*,#3570,.T.);
#4875=ORIENTED_EDGE('',*,*,#3438,.T.);
#4876=ORIENTED_EDGE('',*,*,#3435,.T.);
#4877=ORIENTED_EDGE('',*,*,#3432,.T.);
#4878=ORIENTED_EDGE('',*,*,#3429,.T.);
#4879=ORIENTED_EDGE('',*,*,#3426,.T.);
#4880=ORIENTED_EDGE('',*,*,#3423,.T.);
#4881=ORIENTED_EDGE('',*,*,#3420,.T.);
#4882=ORIENTED_EDGE('',*,*,#3413,.T.);
#4883=ORIENTED_EDGE('',*,*,#3561,.T.);
#4884=ORIENTED_EDGE('',*,*,#3410,.F.);
#4885=ORIENTED_EDGE('',*,*,#3560,.T.);
#4886=ORIENTED_EDGE('',*,*,#3387,.T.);
#4887=ORIENTED_EDGE('',*,*,#3567,.T.);
#4888=ORIENTED_EDGE('',*,*,#3384,.F.);
#4889=ORIENTED_EDGE('',*,*,#3566,.T.);
#4890=ORIENTED_EDGE('',*,*,#3361,.T.);
#4891=ORIENTED_EDGE('',*,*,#3573,.T.);
#4892=ORIENTED_EDGE('',*,*,#3358,.F.);
#4893=ORIENTED_EDGE('',*,*,#3572,.T.);
#4894=ORIENTED_EDGE('',*,*,#3335,.T.);
#4895=ORIENTED_EDGE('',*,*,#3547,.T.);
#4896=ORIENTED_EDGE('',*,*,#3332,.F.);
#4897=ORIENTED_EDGE('',*,*,#3545,.T.);
#4898=ORIENTED_EDGE('',*,*,#3575,.F.);
#4899=ORIENTED_EDGE('',*,*,#3576,.T.);
#4900=ORIENTED_EDGE('',*,*,#3577,.F.);
#4901=ORIENTED_EDGE('',*,*,#3576,.F.);
#4902=ORIENTED_EDGE('',*,*,#3578,.F.);
#4903=ORIENTED_EDGE('',*,*,#3579,.T.);
#4904=ORIENTED_EDGE('',*,*,#3580,.F.);
#4905=ORIENTED_EDGE('',*,*,#3579,.F.);
#4906=ORIENTED_EDGE('',*,*,#3581,.F.);
#4907=ORIENTED_EDGE('',*,*,#3582,.T.);
#4908=ORIENTED_EDGE('',*,*,#3583,.F.);
#4909=ORIENTED_EDGE('',*,*,#3582,.F.);
#4910=ORIENTED_EDGE('',*,*,#3584,.F.);
#4911=ORIENTED_EDGE('',*,*,#3585,.T.);
#4912=ORIENTED_EDGE('',*,*,#3586,.F.);
#4913=ORIENTED_EDGE('',*,*,#3585,.F.);
#4914=ORIENTED_EDGE('',*,*,#3587,.T.);
#4915=ORIENTED_EDGE('',*,*,#3588,.F.);
#4916=ORIENTED_EDGE('',*,*,#3584,.T.);
#4917=ORIENTED_EDGE('',*,*,#3581,.T.);
#4918=ORIENTED_EDGE('',*,*,#3578,.T.);
#4919=ORIENTED_EDGE('',*,*,#3575,.T.);
#4920=ORIENTED_EDGE('',*,*,#3587,.F.);
#4921=ORIENTED_EDGE('',*,*,#3589,.T.);
#4922=ORIENTED_EDGE('',*,*,#3590,.T.);
#4923=ORIENTED_EDGE('',*,*,#3589,.F.);
#4924=ORIENTED_EDGE('',*,*,#3590,.F.);
#4925=ORIENTED_EDGE('',*,*,#3591,.F.);
#4926=ORIENTED_EDGE('',*,*,#3586,.T.);
#4927=ORIENTED_EDGE('',*,*,#3583,.T.);
#4928=ORIENTED_EDGE('',*,*,#3580,.T.);
#4929=ORIENTED_EDGE('',*,*,#3577,.T.);
#4930=ORIENTED_EDGE('',*,*,#3550,.F.);
#4931=ORIENTED_EDGE('',*,*,#3592,.T.);
#4932=ORIENTED_EDGE('',*,*,#3588,.T.);
#4933=ORIENTED_EDGE('',*,*,#3592,.F.);
#4934=ORIENTED_EDGE('',*,*,#3593,.F.);
#4935=ORIENTED_EDGE('',*,*,#3531,.F.);
#4936=ORIENTED_EDGE('',*,*,#3594,.F.);
#4937=ORIENTED_EDGE('',*,*,#3595,.T.);
#4938=ORIENTED_EDGE('',*,*,#3596,.F.);
#4939=ORIENTED_EDGE('',*,*,#3597,.T.);
#4940=ORIENTED_EDGE('',*,*,#3598,.F.);
#4941=ORIENTED_EDGE('',*,*,#3536,.F.);
#4942=ORIENTED_EDGE('',*,*,#3599,.F.);
#4943=ORIENTED_EDGE('',*,*,#3535,.F.);
#4944=ORIENTED_EDGE('',*,*,#3600,.F.);
#4945=ORIENTED_EDGE('',*,*,#3601,.T.);
#4946=ORIENTED_EDGE('',*,*,#3602,.F.);
#4947=ORIENTED_EDGE('',*,*,#3603,.T.);
#4948=ORIENTED_EDGE('',*,*,#3604,.F.);
#4949=ORIENTED_EDGE('',*,*,#3529,.F.);
#4950=ORIENTED_EDGE('',*,*,#3596,.T.);
#4951=ORIENTED_EDGE('',*,*,#3539,.F.);
#4952=ORIENTED_EDGE('',*,*,#3605,.T.);
#4953=ORIENTED_EDGE('',*,*,#3606,.F.);
#4954=ORIENTED_EDGE('',*,*,#3607,.T.);
#4955=ORIENTED_EDGE('',*,*,#3532,.F.);
#4956=ORIENTED_EDGE('',*,*,#3599,.T.);
#4957=ORIENTED_EDGE('',*,*,#3608,.F.);
#4958=ORIENTED_EDGE('',*,*,#3602,.T.);
#4959=ORIENTED_EDGE('',*,*,#3528,.F.);
#4960=ORIENTED_EDGE('',*,*,#3609,.T.);
#4961=ORIENTED_EDGE('',*,*,#3591,.T.);
#4962=ORIENTED_EDGE('',*,*,#3609,.F.);
#4963=ORIENTED_EDGE('',*,*,#3527,.F.);
#4964=ORIENTED_EDGE('',*,*,#3593,.T.);
#4965=ORIENTED_EDGE('',*,*,#3610,.F.);
#4966=ORIENTED_EDGE('',*,*,#3606,.T.);
#4967=ORIENTED_EDGE('',*,*,#3611,.F.);
#4968=ORIENTED_EDGE('',*,*,#3612,.F.);
#4969=ORIENTED_EDGE('',*,*,#3597,.F.);
#4970=ORIENTED_EDGE('',*,*,#3610,.T.);
#4971=ORIENTED_EDGE('',*,*,#3595,.F.);
#4972=ORIENTED_EDGE('',*,*,#3613,.F.);
#4973=ORIENTED_EDGE('',*,*,#3603,.F.);
#4974=ORIENTED_EDGE('',*,*,#3608,.T.);
#4975=ORIENTED_EDGE('',*,*,#3601,.F.);
#4976=ORIENTED_EDGE('',*,*,#3614,.F.);
#4977=ORIENTED_EDGE('',*,*,#3615,.F.);
#4978=ORIENTED_EDGE('',*,*,#3616,.F.);
#4979=ORIENTED_EDGE('',*,*,#3600,.T.);
#4980=ORIENTED_EDGE('',*,*,#3534,.F.);
#4981=ORIENTED_EDGE('',*,*,#3617,.F.);
#4982=ORIENTED_EDGE('',*,*,#3614,.T.);
#4983=ORIENTED_EDGE('',*,*,#3594,.T.);
#4984=ORIENTED_EDGE('',*,*,#3530,.F.);
#4985=ORIENTED_EDGE('',*,*,#3604,.T.);
#4986=ORIENTED_EDGE('',*,*,#3613,.T.);
#4987=ORIENTED_EDGE('',*,*,#3540,.F.);
#4988=ORIENTED_EDGE('',*,*,#3618,.T.);
#4989=ORIENTED_EDGE('',*,*,#3616,.T.);
#4990=ORIENTED_EDGE('',*,*,#3618,.F.);
#4991=ORIENTED_EDGE('',*,*,#3598,.T.);
#4992=ORIENTED_EDGE('',*,*,#3612,.T.);
#4993=ORIENTED_EDGE('',*,*,#3619,.F.);
#4994=ORIENTED_EDGE('',*,*,#3537,.F.);
#4995=ORIENTED_EDGE('',*,*,#3617,.T.);
#4996=ORIENTED_EDGE('',*,*,#3533,.F.);
#4997=ORIENTED_EDGE('',*,*,#3607,.F.);
#4998=ORIENTED_EDGE('',*,*,#3615,.T.);
#4999=ORIENTED_EDGE('',*,*,#3620,.T.);
#5000=ORIENTED_EDGE('',*,*,#3548,.T.);
#5001=ORIENTED_EDGE('',*,*,#3337,.T.);
#5002=ORIENTED_EDGE('',*,*,#3544,.T.);
#5003=ORIENTED_EDGE('',*,*,#3519,.T.);
#5004=ORIENTED_EDGE('',*,*,#3568,.T.);
#5005=ORIENTED_EDGE('',*,*,#3389,.T.);
#5006=ORIENTED_EDGE('',*,*,#3565,.T.);
#5007=ORIENTED_EDGE('',*,*,#3467,.T.);
#5008=ORIENTED_EDGE('',*,*,#3574,.T.);
#5009=ORIENTED_EDGE('',*,*,#3363,.T.);
#5010=ORIENTED_EDGE('',*,*,#3571,.T.);
#5011=ORIENTED_EDGE('',*,*,#3441,.T.);
#5012=ORIENTED_EDGE('',*,*,#3562,.T.);
#5013=ORIENTED_EDGE('',*,*,#3415,.T.);
#5014=ORIENTED_EDGE('',*,*,#3559,.T.);
#5015=ORIENTED_EDGE('',*,*,#3493,.T.);
#5016=ORIENTED_EDGE('',*,*,#3524,.T.);
#5017=ORIENTED_EDGE('',*,*,#3619,.T.);
#5018=ORIENTED_EDGE('',*,*,#3611,.T.);
#5019=ORIENTED_EDGE('',*,*,#3605,.F.);
#5020=ORIENTED_EDGE('',*,*,#3538,.F.);
#5021=ORIENTED_EDGE('',*,*,#3620,.F.);
#5022=ORIENTED_EDGE('',*,*,#3621,.T.);
#5023=ORIENTED_EDGE('',*,*,#3549,.T.);
#5024=ORIENTED_EDGE('',*,*,#3621,.F.);
#5025=ORIENTED_EDGE('',*,*,#3622,.T.);
#5026=ORIENTED_EDGE('',*,*,#3623,.T.);
#5027=ORIENTED_EDGE('',*,*,#3622,.F.);
#5028=ORIENTED_EDGE('',*,*,#3623,.F.);
#5029=ORIENTED_EDGE('',*,*,#3624,.T.);
#5030=ORIENTED_EDGE('',*,*,#3625,.T.);
#5031=ORIENTED_EDGE('',*,*,#3626,.T.);
#5032=ORIENTED_EDGE('',*,*,#3627,.T.);
#5033=ORIENTED_EDGE('',*,*,#3628,.T.);
#5034=ORIENTED_EDGE('',*,*,#3629,.T.);
#5035=ORIENTED_EDGE('',*,*,#3627,.F.);
#5036=ORIENTED_EDGE('',*,*,#3630,.T.);
#5037=ORIENTED_EDGE('',*,*,#3631,.F.);
#5038=ORIENTED_EDGE('',*,*,#3630,.F.);
#5039=ORIENTED_EDGE('',*,*,#3629,.F.);
#5040=ORIENTED_EDGE('',*,*,#3632,.T.);
#5041=ORIENTED_EDGE('',*,*,#3633,.F.);
#5042=ORIENTED_EDGE('',*,*,#3632,.F.);
#5043=ORIENTED_EDGE('',*,*,#3625,.F.);
#5044=ORIENTED_EDGE('',*,*,#3634,.T.);
#5045=ORIENTED_EDGE('',*,*,#3635,.F.);
#5046=ORIENTED_EDGE('',*,*,#3634,.F.);
#5047=ORIENTED_EDGE('',*,*,#3626,.F.);
#5048=ORIENTED_EDGE('',*,*,#3636,.T.);
#5049=ORIENTED_EDGE('',*,*,#3637,.F.);
#5050=ORIENTED_EDGE('',*,*,#3636,.F.);
#5051=ORIENTED_EDGE('',*,*,#3638,.F.);
#5052=ORIENTED_EDGE('',*,*,#3631,.T.);
#5053=ORIENTED_EDGE('',*,*,#3633,.T.);
#5054=ORIENTED_EDGE('',*,*,#3635,.T.);
#5055=ORIENTED_EDGE('',*,*,#3637,.T.);
#5056=ORIENTED_EDGE('',*,*,#3639,.T.);
#5057=ORIENTED_EDGE('',*,*,#3624,.F.);
#5058=ORIENTED_EDGE('',*,*,#3640,.T.);
#5059=ORIENTED_EDGE('',*,*,#3638,.T.);
#5060=ORIENTED_EDGE('',*,*,#3640,.F.);
#5061=ORIENTED_EDGE('',*,*,#3641,.F.);
#5062=ORIENTED_EDGE('',*,*,#3642,.F.);
#5063=ORIENTED_EDGE('',*,*,#3643,.F.);
#5064=ORIENTED_EDGE('',*,*,#3628,.F.);
#5065=ORIENTED_EDGE('',*,*,#3644,.T.);
#5066=ORIENTED_EDGE('',*,*,#3643,.T.);
#5067=ORIENTED_EDGE('',*,*,#3644,.F.);
#5068=ORIENTED_EDGE('',*,*,#3639,.F.);
#5069=ORIENTED_EDGE('',*,*,#3645,.T.);
#5070=ORIENTED_EDGE('',*,*,#3646,.F.);
#5071=ORIENTED_EDGE('',*,*,#3647,.F.);
#5072=ORIENTED_EDGE('',*,*,#3645,.F.);
#5073=ORIENTED_EDGE('',*,*,#3648,.F.);
#5074=ORIENTED_EDGE('',*,*,#3642,.T.);
#5075=ORIENTED_EDGE('',*,*,#3649,.F.);
#5076=ORIENTED_EDGE('',*,*,#3650,.F.);
#5077=ORIENTED_EDGE('',*,*,#3650,.T.);
#5078=ORIENTED_EDGE('',*,*,#3651,.F.);
#5079=ORIENTED_EDGE('',*,*,#3652,.T.);
#5080=ORIENTED_EDGE('',*,*,#3653,.T.);
#5081=ORIENTED_EDGE('',*,*,#3652,.F.);
#5082=ORIENTED_EDGE('',*,*,#3654,.F.);
#5083=ORIENTED_EDGE('',*,*,#3655,.F.);
#5084=ORIENTED_EDGE('',*,*,#3656,.T.);
#5085=ORIENTED_EDGE('',*,*,#3657,.T.);
#5086=ORIENTED_EDGE('',*,*,#3656,.F.);
#5087=ORIENTED_EDGE('',*,*,#3646,.T.);
#5088=ORIENTED_EDGE('',*,*,#3647,.T.);
#5089=ORIENTED_EDGE('',*,*,#3658,.F.);
#5090=ORIENTED_EDGE('',*,*,#3659,.T.);
#5091=ORIENTED_EDGE('',*,*,#3660,.F.);
#5092=ORIENTED_EDGE('',*,*,#3659,.F.);
#5093=ORIENTED_EDGE('',*,*,#3661,.F.);
#5094=ORIENTED_EDGE('',*,*,#3662,.T.);
#5095=ORIENTED_EDGE('',*,*,#3663,.F.);
#5096=ORIENTED_EDGE('',*,*,#3662,.F.);
#5097=ORIENTED_EDGE('',*,*,#3664,.F.);
#5098=ORIENTED_EDGE('',*,*,#3665,.T.);
#5099=ORIENTED_EDGE('',*,*,#3666,.F.);
#5100=ORIENTED_EDGE('',*,*,#3665,.F.);
#5101=ORIENTED_EDGE('',*,*,#3667,.F.);
#5102=ORIENTED_EDGE('',*,*,#3668,.T.);
#5103=ORIENTED_EDGE('',*,*,#3669,.F.);
#5104=ORIENTED_EDGE('',*,*,#3668,.F.);
#5105=ORIENTED_EDGE('',*,*,#3670,.F.);
#5106=ORIENTED_EDGE('',*,*,#3671,.T.);
#5107=ORIENTED_EDGE('',*,*,#3672,.T.);
#5108=ORIENTED_EDGE('',*,*,#3671,.F.);
#5109=ORIENTED_EDGE('',*,*,#3673,.F.);
#5110=ORIENTED_EDGE('',*,*,#3672,.F.);
#5111=ORIENTED_EDGE('',*,*,#3674,.F.);
#5112=ORIENTED_EDGE('',*,*,#3675,.T.);
#5113=ORIENTED_EDGE('',*,*,#3675,.F.);
#5114=ORIENTED_EDGE('',*,*,#3676,.T.);
#5115=ORIENTED_EDGE('',*,*,#3677,.T.);
#5116=ORIENTED_EDGE('',*,*,#3676,.F.);
#5117=ORIENTED_EDGE('',*,*,#3678,.F.);
#5118=ORIENTED_EDGE('',*,*,#3679,.T.);
#5119=ORIENTED_EDGE('',*,*,#3673,.T.);
#5120=ORIENTED_EDGE('',*,*,#3679,.F.);
#5121=ORIENTED_EDGE('',*,*,#3670,.T.);
#5122=ORIENTED_EDGE('',*,*,#3677,.F.);
#5123=ORIENTED_EDGE('',*,*,#3648,.T.);
#5124=ORIENTED_EDGE('',*,*,#3654,.T.);
#5125=ORIENTED_EDGE('',*,*,#3651,.T.);
#5126=ORIENTED_EDGE('',*,*,#3649,.T.);
#5127=ORIENTED_EDGE('',*,*,#3641,.T.);
#5128=ORIENTED_EDGE('',*,*,#3678,.T.);
#5129=ORIENTED_EDGE('',*,*,#3680,.F.);
#5130=ORIENTED_EDGE('',*,*,#3681,.T.);
#5131=ORIENTED_EDGE('',*,*,#3674,.T.);
#5132=ORIENTED_EDGE('',*,*,#3681,.F.);
#5133=ORIENTED_EDGE('',*,*,#3655,.T.);
#5134=ORIENTED_EDGE('',*,*,#3680,.T.);
#5135=ORIENTED_EDGE('',*,*,#3667,.T.);
#5136=ORIENTED_EDGE('',*,*,#3664,.T.);
#5137=ORIENTED_EDGE('',*,*,#3661,.T.);
#5138=ORIENTED_EDGE('',*,*,#3658,.T.);
#5139=ORIENTED_EDGE('',*,*,#3657,.F.);
#5140=ORIENTED_EDGE('',*,*,#3653,.F.);
#5141=ORIENTED_EDGE('',*,*,#3669,.T.);
#5142=ORIENTED_EDGE('',*,*,#3666,.T.);
#5143=ORIENTED_EDGE('',*,*,#3663,.T.);
#5144=ORIENTED_EDGE('',*,*,#3660,.T.);
#5145=ORIENTED_EDGE('',*,*,#3682,.F.);
#5146=ORIENTED_EDGE('',*,*,#3683,.F.);
#5147=ORIENTED_EDGE('',*,*,#3684,.T.);
#5148=ORIENTED_EDGE('',*,*,#3685,.F.);
#5149=ORIENTED_EDGE('',*,*,#3686,.F.);
#5150=ORIENTED_EDGE('',*,*,#3687,.F.);
#5151=ORIENTED_EDGE('',*,*,#3688,.F.);
#5152=ORIENTED_EDGE('',*,*,#3689,.T.);
#5153=ORIENTED_EDGE('',*,*,#3690,.F.);
#5154=ORIENTED_EDGE('',*,*,#3684,.F.);
#5155=ORIENTED_EDGE('',*,*,#3691,.T.);
#5156=ORIENTED_EDGE('',*,*,#3692,.T.);
#5157=ORIENTED_EDGE('',*,*,#3693,.F.);
#5158=ORIENTED_EDGE('',*,*,#3692,.F.);
#5159=ORIENTED_EDGE('',*,*,#3694,.F.);
#5160=ORIENTED_EDGE('',*,*,#3695,.T.);
#5161=ORIENTED_EDGE('',*,*,#3696,.F.);
#5162=ORIENTED_EDGE('',*,*,#3695,.F.);
#5163=ORIENTED_EDGE('',*,*,#3697,.T.);
#5164=ORIENTED_EDGE('',*,*,#3687,.T.);
#5165=ORIENTED_EDGE('',*,*,#3683,.T.);
#5166=ORIENTED_EDGE('',*,*,#3688,.T.);
#5167=ORIENTED_EDGE('',*,*,#3697,.F.);
#5168=ORIENTED_EDGE('',*,*,#3694,.T.);
#5169=ORIENTED_EDGE('',*,*,#3691,.F.);
#5170=ORIENTED_EDGE('',*,*,#3698,.F.);
#5171=ORIENTED_EDGE('',*,*,#3685,.T.);
#5172=ORIENTED_EDGE('',*,*,#3690,.T.);
#5173=ORIENTED_EDGE('',*,*,#3693,.T.);
#5174=ORIENTED_EDGE('',*,*,#3696,.T.);
#5175=ORIENTED_EDGE('',*,*,#3686,.T.);
#5176=ORIENTED_EDGE('',*,*,#3699,.F.);
#5177=ORIENTED_EDGE('',*,*,#3700,.T.);
#5178=ORIENTED_EDGE('',*,*,#3701,.T.);
#5179=ORIENTED_EDGE('',*,*,#3700,.F.);
#5180=ORIENTED_EDGE('',*,*,#3702,.F.);
#5181=ORIENTED_EDGE('',*,*,#3703,.F.);
#5182=ORIENTED_EDGE('',*,*,#3704,.T.);
#5183=ORIENTED_EDGE('',*,*,#3705,.T.);
#5184=ORIENTED_EDGE('',*,*,#3706,.F.);
#5185=ORIENTED_EDGE('',*,*,#3705,.F.);
#5186=ORIENTED_EDGE('',*,*,#3707,.F.);
#5187=ORIENTED_EDGE('',*,*,#3708,.T.);
#5188=ORIENTED_EDGE('',*,*,#3709,.F.);
#5189=ORIENTED_EDGE('',*,*,#3708,.F.);
#5190=ORIENTED_EDGE('',*,*,#3710,.T.);
#5191=ORIENTED_EDGE('',*,*,#3711,.T.);
#5192=ORIENTED_EDGE('',*,*,#3712,.F.);
#5193=ORIENTED_EDGE('',*,*,#3711,.F.);
#5194=ORIENTED_EDGE('',*,*,#3713,.F.);
#5195=ORIENTED_EDGE('',*,*,#3703,.T.);
#5196=ORIENTED_EDGE('',*,*,#3707,.T.);
#5197=ORIENTED_EDGE('',*,*,#3704,.F.);
#5198=ORIENTED_EDGE('',*,*,#3713,.T.);
#5199=ORIENTED_EDGE('',*,*,#3710,.F.);
#5200=ORIENTED_EDGE('',*,*,#3714,.F.);
#5201=ORIENTED_EDGE('',*,*,#3715,.F.);
#5202=ORIENTED_EDGE('',*,*,#3716,.T.);
#5203=ORIENTED_EDGE('',*,*,#3717,.T.);
#5204=ORIENTED_EDGE('',*,*,#3718,.F.);
#5205=ORIENTED_EDGE('',*,*,#3717,.F.);
#5206=ORIENTED_EDGE('',*,*,#3719,.F.);
#5207=ORIENTED_EDGE('',*,*,#3720,.T.);
#5208=ORIENTED_EDGE('',*,*,#3721,.F.);
#5209=ORIENTED_EDGE('',*,*,#3720,.F.);
#5210=ORIENTED_EDGE('',*,*,#3722,.T.);
#5211=ORIENTED_EDGE('',*,*,#3723,.T.);
#5212=ORIENTED_EDGE('',*,*,#3724,.F.);
#5213=ORIENTED_EDGE('',*,*,#3723,.F.);
#5214=ORIENTED_EDGE('',*,*,#3725,.F.);
#5215=ORIENTED_EDGE('',*,*,#3715,.T.);
#5216=ORIENTED_EDGE('',*,*,#3719,.T.);
#5217=ORIENTED_EDGE('',*,*,#3716,.F.);
#5218=ORIENTED_EDGE('',*,*,#3725,.T.);
#5219=ORIENTED_EDGE('',*,*,#3722,.F.);
#5220=ORIENTED_EDGE('',*,*,#3726,.T.);
#5221=ORIENTED_EDGE('',*,*,#3727,.T.);
#5222=ORIENTED_EDGE('',*,*,#3728,.F.);
#5223=ORIENTED_EDGE('',*,*,#3727,.F.);
#5224=ORIENTED_EDGE('',*,*,#3729,.F.);
#5225=ORIENTED_EDGE('',*,*,#3726,.F.);
#5226=ORIENTED_EDGE('',*,*,#3701,.F.);
#5227=ORIENTED_EDGE('',*,*,#3728,.T.);
#5228=ORIENTED_EDGE('',*,*,#3730,.T.);
#5229=ORIENTED_EDGE('',*,*,#3731,.F.);
#5230=ORIENTED_EDGE('',*,*,#3732,.F.);
#5231=ORIENTED_EDGE('',*,*,#3733,.F.);
#5232=ORIENTED_EDGE('',*,*,#3730,.F.);
#5233=ORIENTED_EDGE('',*,*,#3734,.T.);
#5234=ORIENTED_EDGE('',*,*,#3732,.T.);
#5235=ORIENTED_EDGE('',*,*,#3734,.F.);
#5236=ORIENTED_EDGE('',*,*,#3733,.T.);
#5237=ORIENTED_EDGE('',*,*,#3735,.T.);
#5238=ORIENTED_EDGE('',*,*,#3736,.T.);
#5239=ORIENTED_EDGE('',*,*,#3735,.F.);
#5240=ORIENTED_EDGE('',*,*,#3729,.T.);
#5241=ORIENTED_EDGE('',*,*,#3737,.T.);
#5242=ORIENTED_EDGE('',*,*,#3731,.T.);
#5243=ORIENTED_EDGE('',*,*,#3737,.F.);
#5244=ORIENTED_EDGE('',*,*,#3709,.T.);
#5245=ORIENTED_EDGE('',*,*,#3712,.T.);
#5246=ORIENTED_EDGE('',*,*,#3702,.T.);
#5247=ORIENTED_EDGE('',*,*,#3706,.T.);
#5248=ORIENTED_EDGE('',*,*,#3721,.T.);
#5249=ORIENTED_EDGE('',*,*,#3724,.T.);
#5250=ORIENTED_EDGE('',*,*,#3714,.T.);
#5251=ORIENTED_EDGE('',*,*,#3718,.T.);
#5252=ORIENTED_EDGE('',*,*,#3698,.T.);
#5253=ORIENTED_EDGE('',*,*,#3699,.T.);
#5254=ORIENTED_EDGE('',*,*,#3689,.F.);
#5255=ORIENTED_EDGE('',*,*,#3682,.T.);
#5256=ORIENTED_EDGE('',*,*,#3736,.F.);
#5257=ORIENTED_EDGE('',*,*,#3738,.F.);
#5258=ORIENTED_EDGE('',*,*,#3739,.T.);
#5259=ORIENTED_EDGE('',*,*,#3740,.T.);
#5260=ORIENTED_EDGE('',*,*,#3739,.F.);
#5261=ORIENTED_EDGE('',*,*,#3741,.F.);
#5262=ORIENTED_EDGE('',*,*,#3742,.T.);
#5263=ORIENTED_EDGE('',*,*,#3743,.T.);
#5264=ORIENTED_EDGE('',*,*,#3742,.F.);
#5265=ORIENTED_EDGE('',*,*,#3741,.T.);
#5266=ORIENTED_EDGE('',*,*,#3738,.T.);
#5267=ORIENTED_EDGE('',*,*,#3743,.F.);
#5268=ORIENTED_EDGE('',*,*,#3740,.F.);
#5269=ORIENTED_EDGE('',*,*,#3744,.F.);
#5270=ORIENTED_EDGE('',*,*,#3745,.T.);
#5271=ORIENTED_EDGE('',*,*,#3746,.T.);
#5272=ORIENTED_EDGE('',*,*,#3745,.F.);
#5273=ORIENTED_EDGE('',*,*,#3747,.F.);
#5274=ORIENTED_EDGE('',*,*,#3748,.T.);
#5275=ORIENTED_EDGE('',*,*,#3749,.T.);
#5276=ORIENTED_EDGE('',*,*,#3748,.F.);
#5277=ORIENTED_EDGE('',*,*,#3747,.T.);
#5278=ORIENTED_EDGE('',*,*,#3744,.T.);
#5279=ORIENTED_EDGE('',*,*,#3749,.F.);
#5280=ORIENTED_EDGE('',*,*,#3746,.F.);
#5281=ORIENTED_EDGE('',*,*,#3750,.F.);
#5282=ORIENTED_EDGE('',*,*,#3751,.T.);
#5283=ORIENTED_EDGE('',*,*,#3752,.T.);
#5284=ORIENTED_EDGE('',*,*,#3751,.F.);
#5285=ORIENTED_EDGE('',*,*,#3753,.F.);
#5286=ORIENTED_EDGE('',*,*,#3754,.T.);
#5287=ORIENTED_EDGE('',*,*,#3755,.T.);
#5288=ORIENTED_EDGE('',*,*,#3754,.F.);
#5289=ORIENTED_EDGE('',*,*,#3753,.T.);
#5290=ORIENTED_EDGE('',*,*,#3750,.T.);
#5291=ORIENTED_EDGE('',*,*,#3755,.F.);
#5292=ORIENTED_EDGE('',*,*,#3752,.F.);
#5293=ORIENTED_EDGE('',*,*,#3756,.F.);
#5294=ORIENTED_EDGE('',*,*,#3757,.T.);
#5295=ORIENTED_EDGE('',*,*,#3758,.T.);
#5296=ORIENTED_EDGE('',*,*,#3757,.F.);
#5297=ORIENTED_EDGE('',*,*,#3759,.F.);
#5298=ORIENTED_EDGE('',*,*,#3760,.T.);
#5299=ORIENTED_EDGE('',*,*,#3761,.T.);
#5300=ORIENTED_EDGE('',*,*,#3760,.F.);
#5301=ORIENTED_EDGE('',*,*,#3759,.T.);
#5302=ORIENTED_EDGE('',*,*,#3756,.T.);
#5303=ORIENTED_EDGE('',*,*,#3761,.F.);
#5304=ORIENTED_EDGE('',*,*,#3758,.F.);
#5305=ORIENTED_EDGE('',*,*,#3762,.F.);
#5306=ORIENTED_EDGE('',*,*,#3763,.T.);
#5307=ORIENTED_EDGE('',*,*,#3764,.F.);
#5308=ORIENTED_EDGE('',*,*,#3765,.F.);
#5309=ORIENTED_EDGE('',*,*,#3766,.T.);
#5310=ORIENTED_EDGE('',*,*,#3765,.T.);
#5311=ORIENTED_EDGE('',*,*,#3767,.F.);
#5312=ORIENTED_EDGE('',*,*,#3768,.F.);
#5313=ORIENTED_EDGE('',*,*,#3769,.F.);
#5314=ORIENTED_EDGE('',*,*,#3768,.T.);
#5315=ORIENTED_EDGE('',*,*,#3770,.F.);
#5316=ORIENTED_EDGE('',*,*,#3771,.F.);
#5317=ORIENTED_EDGE('',*,*,#3772,.T.);
#5318=ORIENTED_EDGE('',*,*,#3771,.T.);
#5319=ORIENTED_EDGE('',*,*,#3773,.F.);
#5320=ORIENTED_EDGE('',*,*,#3763,.F.);
#5321=ORIENTED_EDGE('',*,*,#3773,.T.);
#5322=ORIENTED_EDGE('',*,*,#3770,.T.);
#5323=ORIENTED_EDGE('',*,*,#3767,.T.);
#5324=ORIENTED_EDGE('',*,*,#3764,.T.);
#5325=ORIENTED_EDGE('',*,*,#3772,.F.);
#5326=ORIENTED_EDGE('',*,*,#3762,.T.);
#5327=ORIENTED_EDGE('',*,*,#3766,.F.);
#5328=ORIENTED_EDGE('',*,*,#3769,.T.);
#5329=ORIENTED_EDGE('',*,*,#3774,.F.);
#5330=ORIENTED_EDGE('',*,*,#3775,.T.);
#5331=ORIENTED_EDGE('',*,*,#3776,.T.);
#5332=ORIENTED_EDGE('',*,*,#3775,.F.);
#5333=ORIENTED_EDGE('',*,*,#3777,.F.);
#5334=ORIENTED_EDGE('',*,*,#3778,.T.);
#5335=ORIENTED_EDGE('',*,*,#3779,.T.);
#5336=ORIENTED_EDGE('',*,*,#3778,.F.);
#5337=ORIENTED_EDGE('',*,*,#3777,.T.);
#5338=ORIENTED_EDGE('',*,*,#3774,.T.);
#5339=ORIENTED_EDGE('',*,*,#3779,.F.);
#5340=ORIENTED_EDGE('',*,*,#3776,.F.);
#5341=ORIENTED_EDGE('',*,*,#3780,.F.);
#5342=ORIENTED_EDGE('',*,*,#3781,.T.);
#5343=ORIENTED_EDGE('',*,*,#3782,.T.);
#5344=ORIENTED_EDGE('',*,*,#3781,.F.);
#5345=ORIENTED_EDGE('',*,*,#3783,.F.);
#5346=ORIENTED_EDGE('',*,*,#3784,.T.);
#5347=ORIENTED_EDGE('',*,*,#3785,.T.);
#5348=ORIENTED_EDGE('',*,*,#3784,.F.);
#5349=ORIENTED_EDGE('',*,*,#3783,.T.);
#5350=ORIENTED_EDGE('',*,*,#3780,.T.);
#5351=ORIENTED_EDGE('',*,*,#3785,.F.);
#5352=ORIENTED_EDGE('',*,*,#3782,.F.);
#5353=ORIENTED_EDGE('',*,*,#3786,.F.);
#5354=ORIENTED_EDGE('',*,*,#3787,.T.);
#5355=ORIENTED_EDGE('',*,*,#3788,.T.);
#5356=ORIENTED_EDGE('',*,*,#3787,.F.);
#5357=ORIENTED_EDGE('',*,*,#3789,.F.);
#5358=ORIENTED_EDGE('',*,*,#3790,.T.);
#5359=ORIENTED_EDGE('',*,*,#3791,.T.);
#5360=ORIENTED_EDGE('',*,*,#3790,.F.);
#5361=ORIENTED_EDGE('',*,*,#3789,.T.);
#5362=ORIENTED_EDGE('',*,*,#3786,.T.);
#5363=ORIENTED_EDGE('',*,*,#3791,.F.);
#5364=ORIENTED_EDGE('',*,*,#3788,.F.);
#5365=ORIENTED_EDGE('',*,*,#3792,.F.);
#5366=ORIENTED_EDGE('',*,*,#3793,.T.);
#5367=ORIENTED_EDGE('',*,*,#3794,.T.);
#5368=ORIENTED_EDGE('',*,*,#3793,.F.);
#5369=ORIENTED_EDGE('',*,*,#3795,.F.);
#5370=ORIENTED_EDGE('',*,*,#3796,.T.);
#5371=ORIENTED_EDGE('',*,*,#3797,.T.);
#5372=ORIENTED_EDGE('',*,*,#3796,.F.);
#5373=ORIENTED_EDGE('',*,*,#3795,.T.);
#5374=ORIENTED_EDGE('',*,*,#3792,.T.);
#5375=ORIENTED_EDGE('',*,*,#3797,.F.);
#5376=ORIENTED_EDGE('',*,*,#3794,.F.);
#5377=ORIENTED_EDGE('',*,*,#3798,.F.);
#5378=ORIENTED_EDGE('',*,*,#3799,.F.);
#5379=ORIENTED_EDGE('',*,*,#3800,.F.);
#5380=ORIENTED_EDGE('',*,*,#3801,.F.);
#5381=ORIENTED_EDGE('',*,*,#3802,.F.);
#5382=ORIENTED_EDGE('',*,*,#3803,.F.);
#5383=ORIENTED_EDGE('',*,*,#3804,.F.);
#5384=ORIENTED_EDGE('',*,*,#3805,.F.);
#5385=ORIENTED_EDGE('',*,*,#3805,.T.);
#5386=ORIENTED_EDGE('',*,*,#3806,.F.);
#5387=ORIENTED_EDGE('',*,*,#3799,.T.);
#5388=ORIENTED_EDGE('',*,*,#3807,.F.);
#5389=ORIENTED_EDGE('',*,*,#3802,.T.);
#5390=ORIENTED_EDGE('',*,*,#3807,.T.);
#5391=ORIENTED_EDGE('',*,*,#3798,.T.);
#5392=ORIENTED_EDGE('',*,*,#3808,.F.);
#5393=ORIENTED_EDGE('',*,*,#3804,.T.);
#5394=ORIENTED_EDGE('',*,*,#3809,.F.);
#5395=ORIENTED_EDGE('',*,*,#3800,.T.);
#5396=ORIENTED_EDGE('',*,*,#3806,.T.);
#5397=ORIENTED_EDGE('',*,*,#3803,.T.);
#5398=ORIENTED_EDGE('',*,*,#3808,.T.);
#5399=ORIENTED_EDGE('',*,*,#3801,.T.);
#5400=ORIENTED_EDGE('',*,*,#3809,.T.);
#5401=ORIENTED_EDGE('',*,*,#3810,.F.);
#5402=ORIENTED_EDGE('',*,*,#3811,.T.);
#5403=ORIENTED_EDGE('',*,*,#3812,.T.);
#5404=ORIENTED_EDGE('',*,*,#3813,.T.);
#5405=ORIENTED_EDGE('',*,*,#3814,.T.);
#5406=ORIENTED_EDGE('',*,*,#3813,.F.);
#5407=ORIENTED_EDGE('',*,*,#3815,.T.);
#5408=ORIENTED_EDGE('',*,*,#3816,.T.);
#5409=ORIENTED_EDGE('',*,*,#3817,.F.);
#5410=ORIENTED_EDGE('',*,*,#3818,.T.);
#5411=ORIENTED_EDGE('',*,*,#3810,.T.);
#5412=ORIENTED_EDGE('',*,*,#3819,.T.);
#5413=ORIENTED_EDGE('',*,*,#3820,.F.);
#5414=ORIENTED_EDGE('',*,*,#3821,.T.);
#5415=ORIENTED_EDGE('',*,*,#3817,.T.);
#5416=ORIENTED_EDGE('',*,*,#3822,.T.);
#5417=ORIENTED_EDGE('',*,*,#3823,.F.);
#5418=ORIENTED_EDGE('',*,*,#3824,.T.);
#5419=ORIENTED_EDGE('',*,*,#3820,.T.);
#5420=ORIENTED_EDGE('',*,*,#3825,.T.);
#5421=ORIENTED_EDGE('',*,*,#3826,.F.);
#5422=ORIENTED_EDGE('',*,*,#3827,.T.);
#5423=ORIENTED_EDGE('',*,*,#3823,.T.);
#5424=ORIENTED_EDGE('',*,*,#3828,.T.);
#5425=ORIENTED_EDGE('',*,*,#3829,.F.);
#5426=ORIENTED_EDGE('',*,*,#3830,.T.);
#5427=ORIENTED_EDGE('',*,*,#3826,.T.);
#5428=ORIENTED_EDGE('',*,*,#3831,.T.);
#5429=ORIENTED_EDGE('',*,*,#3832,.F.);
#5430=ORIENTED_EDGE('',*,*,#3833,.T.);
#5431=ORIENTED_EDGE('',*,*,#3829,.T.);
#5432=ORIENTED_EDGE('',*,*,#3834,.T.);
#5433=ORIENTED_EDGE('',*,*,#3835,.F.);
#5434=ORIENTED_EDGE('',*,*,#3836,.T.);
#5435=ORIENTED_EDGE('',*,*,#3837,.T.);
#5436=ORIENTED_EDGE('',*,*,#3838,.F.);
#5437=ORIENTED_EDGE('',*,*,#3839,.F.);
#5438=ORIENTED_EDGE('',*,*,#3840,.T.);
#5439=ORIENTED_EDGE('',*,*,#3835,.T.);
#5440=ORIENTED_EDGE('',*,*,#3841,.F.);
#5441=ORIENTED_EDGE('',*,*,#3842,.F.);
#5442=ORIENTED_EDGE('',*,*,#3843,.T.);
#5443=ORIENTED_EDGE('',*,*,#3839,.T.);
#5444=ORIENTED_EDGE('',*,*,#3844,.F.);
#5445=ORIENTED_EDGE('',*,*,#3845,.F.);
#5446=ORIENTED_EDGE('',*,*,#3846,.T.);
#5447=ORIENTED_EDGE('',*,*,#3842,.T.);
#5448=ORIENTED_EDGE('',*,*,#3847,.F.);
#5449=ORIENTED_EDGE('',*,*,#3848,.F.);
#5450=ORIENTED_EDGE('',*,*,#3849,.T.);
#5451=ORIENTED_EDGE('',*,*,#3845,.T.);
#5452=ORIENTED_EDGE('',*,*,#3850,.F.);
#5453=ORIENTED_EDGE('',*,*,#3851,.F.);
#5454=ORIENTED_EDGE('',*,*,#3852,.T.);
#5455=ORIENTED_EDGE('',*,*,#3848,.T.);
#5456=ORIENTED_EDGE('',*,*,#3853,.F.);
#5457=ORIENTED_EDGE('',*,*,#3854,.F.);
#5458=ORIENTED_EDGE('',*,*,#3855,.T.);
#5459=ORIENTED_EDGE('',*,*,#3851,.T.);
#5460=ORIENTED_EDGE('',*,*,#3856,.F.);
#5461=ORIENTED_EDGE('',*,*,#3857,.F.);
#5462=ORIENTED_EDGE('',*,*,#3837,.F.);
#5463=ORIENTED_EDGE('',*,*,#3858,.F.);
#5464=ORIENTED_EDGE('',*,*,#3859,.F.);
#5465=ORIENTED_EDGE('',*,*,#3860,.F.);
#5466=ORIENTED_EDGE('',*,*,#3861,.T.);
#5467=ORIENTED_EDGE('',*,*,#3862,.F.);
#5468=ORIENTED_EDGE('',*,*,#3861,.F.);
#5469=ORIENTED_EDGE('',*,*,#3858,.T.);
#5470=ORIENTED_EDGE('',*,*,#3836,.F.);
#5471=ORIENTED_EDGE('',*,*,#3840,.F.);
#5472=ORIENTED_EDGE('',*,*,#3843,.F.);
#5473=ORIENTED_EDGE('',*,*,#3846,.F.);
#5474=ORIENTED_EDGE('',*,*,#3849,.F.);
#5475=ORIENTED_EDGE('',*,*,#3852,.F.);
#5476=ORIENTED_EDGE('',*,*,#3855,.F.);
#5477=ORIENTED_EDGE('',*,*,#3863,.F.);
#5478=ORIENTED_EDGE('',*,*,#3864,.F.);
#5479=ORIENTED_EDGE('',*,*,#3811,.F.);
#5480=ORIENTED_EDGE('',*,*,#3818,.F.);
#5481=ORIENTED_EDGE('',*,*,#3821,.F.);
#5482=ORIENTED_EDGE('',*,*,#3824,.F.);
#5483=ORIENTED_EDGE('',*,*,#3827,.F.);
#5484=ORIENTED_EDGE('',*,*,#3830,.F.);
#5485=ORIENTED_EDGE('',*,*,#3833,.F.);
#5486=ORIENTED_EDGE('',*,*,#3865,.F.);
#5487=ORIENTED_EDGE('',*,*,#3854,.T.);
#5488=ORIENTED_EDGE('',*,*,#3866,.F.);
#5489=ORIENTED_EDGE('',*,*,#3867,.F.);
#5490=ORIENTED_EDGE('',*,*,#3863,.T.);
#5491=ORIENTED_EDGE('',*,*,#3857,.T.);
#5492=ORIENTED_EDGE('',*,*,#3860,.T.);
#5493=ORIENTED_EDGE('',*,*,#3868,.F.);
#5494=ORIENTED_EDGE('',*,*,#3834,.F.);
#5495=ORIENTED_EDGE('',*,*,#3831,.F.);
#5496=ORIENTED_EDGE('',*,*,#3828,.F.);
#5497=ORIENTED_EDGE('',*,*,#3825,.F.);
#5498=ORIENTED_EDGE('',*,*,#3822,.F.);
#5499=ORIENTED_EDGE('',*,*,#3819,.F.);
#5500=ORIENTED_EDGE('',*,*,#3816,.F.);
#5501=ORIENTED_EDGE('',*,*,#3869,.F.);
#5502=ORIENTED_EDGE('',*,*,#3866,.T.);
#5503=ORIENTED_EDGE('',*,*,#3856,.T.);
#5504=ORIENTED_EDGE('',*,*,#3853,.T.);
#5505=ORIENTED_EDGE('',*,*,#3850,.T.);
#5506=ORIENTED_EDGE('',*,*,#3847,.T.);
#5507=ORIENTED_EDGE('',*,*,#3844,.T.);
#5508=ORIENTED_EDGE('',*,*,#3841,.T.);
#5509=ORIENTED_EDGE('',*,*,#3838,.T.);
#5510=ORIENTED_EDGE('',*,*,#3812,.F.);
#5511=ORIENTED_EDGE('',*,*,#3864,.T.);
#5512=ORIENTED_EDGE('',*,*,#3867,.T.);
#5513=ORIENTED_EDGE('',*,*,#3869,.T.);
#5514=ORIENTED_EDGE('',*,*,#3815,.F.);
#5515=ORIENTED_EDGE('',*,*,#3832,.T.);
#5516=ORIENTED_EDGE('',*,*,#3868,.T.);
#5517=ORIENTED_EDGE('',*,*,#3859,.T.);
#5518=ORIENTED_EDGE('',*,*,#3865,.T.);
#5519=ORIENTED_EDGE('',*,*,#3870,.F.);
#5520=ORIENTED_EDGE('',*,*,#3871,.T.);
#5521=ORIENTED_EDGE('',*,*,#3872,.T.);
#5522=ORIENTED_EDGE('',*,*,#3873,.F.);
#5523=ORIENTED_EDGE('',*,*,#3874,.F.);
#5524=ORIENTED_EDGE('',*,*,#3875,.T.);
#5525=ORIENTED_EDGE('',*,*,#3876,.T.);
#5526=ORIENTED_EDGE('',*,*,#3871,.F.);
#5527=ORIENTED_EDGE('',*,*,#3877,.F.);
#5528=ORIENTED_EDGE('',*,*,#3878,.T.);
#5529=ORIENTED_EDGE('',*,*,#3879,.T.);
#5530=ORIENTED_EDGE('',*,*,#3875,.F.);
#5531=ORIENTED_EDGE('',*,*,#3880,.F.);
#5532=ORIENTED_EDGE('',*,*,#3881,.T.);
#5533=ORIENTED_EDGE('',*,*,#3882,.T.);
#5534=ORIENTED_EDGE('',*,*,#3878,.F.);
#5535=ORIENTED_EDGE('',*,*,#3883,.F.);
#5536=ORIENTED_EDGE('',*,*,#3884,.T.);
#5537=ORIENTED_EDGE('',*,*,#3885,.T.);
#5538=ORIENTED_EDGE('',*,*,#3881,.F.);
#5539=ORIENTED_EDGE('',*,*,#3886,.F.);
#5540=ORIENTED_EDGE('',*,*,#3873,.T.);
#5541=ORIENTED_EDGE('',*,*,#3887,.T.);
#5542=ORIENTED_EDGE('',*,*,#3884,.F.);
#5543=ORIENTED_EDGE('',*,*,#3887,.F.);
#5544=ORIENTED_EDGE('',*,*,#3872,.F.);
#5545=ORIENTED_EDGE('',*,*,#3876,.F.);
#5546=ORIENTED_EDGE('',*,*,#3879,.F.);
#5547=ORIENTED_EDGE('',*,*,#3882,.F.);
#5548=ORIENTED_EDGE('',*,*,#3885,.F.);
#5549=ORIENTED_EDGE('',*,*,#3888,.T.);
#5550=ORIENTED_EDGE('',*,*,#3814,.F.);
#5551=ORIENTED_EDGE('',*,*,#3888,.F.);
#5552=ORIENTED_EDGE('',*,*,#3889,.T.);
#5553=ORIENTED_EDGE('',*,*,#3890,.T.);
#5554=ORIENTED_EDGE('',*,*,#3889,.F.);
#5555=ORIENTED_EDGE('',*,*,#3890,.F.);
#5556=ORIENTED_EDGE('',*,*,#3870,.T.);
#5557=ORIENTED_EDGE('',*,*,#3886,.T.);
#5558=ORIENTED_EDGE('',*,*,#3883,.T.);
#5559=ORIENTED_EDGE('',*,*,#3880,.T.);
#5560=ORIENTED_EDGE('',*,*,#3877,.T.);
#5561=ORIENTED_EDGE('',*,*,#3874,.T.);
#5562=ORIENTED_EDGE('',*,*,#3862,.T.);
#5563=CYLINDRICAL_SURFACE('',#6343,6.35);
#5564=CYLINDRICAL_SURFACE('',#6346,6.85);
#5565=CYLINDRICAL_SURFACE('',#6352,0.35);
#5566=CYLINDRICAL_SURFACE('',#6355,0.35);
#5567=CYLINDRICAL_SURFACE('',#6358,0.35);
#5568=CYLINDRICAL_SURFACE('',#6361,0.35);
#5569=CYLINDRICAL_SURFACE('',#6365,2.9);
#5570=CYLINDRICAL_SURFACE('',#6369,3.2);
#5571=CYLINDRICAL_SURFACE('',#6374,2.9);
#5572=CYLINDRICAL_SURFACE('',#6378,3.2);
#5573=CYLINDRICAL_SURFACE('',#6383,2.9);
#5574=CYLINDRICAL_SURFACE('',#6387,3.2);
#5575=CYLINDRICAL_SURFACE('',#6392,2.9);
#5576=CYLINDRICAL_SURFACE('',#6396,3.2);
#5577=CYLINDRICAL_SURFACE('',#6401,2.9);
#5578=CYLINDRICAL_SURFACE('',#6405,3.2);
#5579=CYLINDRICAL_SURFACE('',#6410,2.9);
#5580=CYLINDRICAL_SURFACE('',#6414,3.2);
#5581=CYLINDRICAL_SURFACE('',#6430,5.8);
#5582=CYLINDRICAL_SURFACE('',#6432,5.8);
#5583=CYLINDRICAL_SURFACE('',#6434,5.8);
#5584=CYLINDRICAL_SURFACE('',#6436,1.7);
#5585=CYLINDRICAL_SURFACE('',#6444,6.2);
#5586=CYLINDRICAL_SURFACE('',#6446,8.2);
#5587=CYLINDRICAL_SURFACE('',#6452,6.35);
#5588=CYLINDRICAL_SURFACE('',#6455,6.85);
#5589=CYLINDRICAL_SURFACE('',#6461,0.35);
#5590=CYLINDRICAL_SURFACE('',#6464,0.35);
#5591=CYLINDRICAL_SURFACE('',#6467,0.35);
#5592=CYLINDRICAL_SURFACE('',#6470,0.35);
#5593=CYLINDRICAL_SURFACE('',#6473,2.7);
#5594=CYLINDRICAL_SURFACE('',#6475,8.2);
#5595=CYLINDRICAL_SURFACE('',#6502,2.9);
#5596=CYLINDRICAL_SURFACE('',#6505,3.2);
#5597=CYLINDRICAL_SURFACE('',#6509,2.9);
#5598=CYLINDRICAL_SURFACE('',#6512,3.2);
#5599=CYLINDRICAL_SURFACE('',#6516,2.9);
#5600=CYLINDRICAL_SURFACE('',#6519,3.2);
#5601=CYLINDRICAL_SURFACE('',#6523,2.9);
#5602=CYLINDRICAL_SURFACE('',#6526,3.2);
#5603=CYLINDRICAL_SURFACE('',#6530,2.9);
#5604=CYLINDRICAL_SURFACE('',#6533,3.2);
#5605=CYLINDRICAL_SURFACE('',#6537,2.9);
#5606=CYLINDRICAL_SURFACE('',#6540,3.2);
#5607=CYLINDRICAL_SURFACE('',#6544,1.5);
#5608=CYLINDRICAL_SURFACE('',#6549,1.);
#5609=CYLINDRICAL_SURFACE('',#6550,5.);
#5610=CYLINDRICAL_SURFACE('',#6554,1.5);
#5611=CYLINDRICAL_SURFACE('',#6557,1.7);
#5612=CYLINDRICAL_SURFACE('',#6563,0.25175);
#5613=CYLINDRICAL_SURFACE('',#6565,0.25175);
#5614=CYLINDRICAL_SURFACE('',#6566,0.25175);
#5615=CYLINDRICAL_SURFACE('',#6567,0.25175);
#5616=CYLINDRICAL_SURFACE('',#6568,0.25175);
#5617=CYLINDRICAL_SURFACE('',#6569,0.25175);
#5618=CYLINDRICAL_SURFACE('',#6570,0.25175);
#5619=CYLINDRICAL_SURFACE('',#6571,0.25175);
#5620=CYLINDRICAL_SURFACE('',#6573,0.25175);
#5621=CYLINDRICAL_SURFACE('',#6575,0.25175);
#5622=CYLINDRICAL_SURFACE('',#6576,0.25175);
#5623=CYLINDRICAL_SURFACE('',#6577,0.25175);
#5624=CYLINDRICAL_SURFACE('',#6578,0.25175);
#5625=CYLINDRICAL_SURFACE('',#6579,0.25175);
#5626=CYLINDRICAL_SURFACE('',#6580,0.25175);
#5627=CYLINDRICAL_SURFACE('',#6581,0.25175);
#5628=CYLINDRICAL_SURFACE('',#6583,0.25175);
#5629=CYLINDRICAL_SURFACE('',#6585,0.25175);
#5630=CYLINDRICAL_SURFACE('',#6586,0.25175);
#5631=CYLINDRICAL_SURFACE('',#6587,0.25175);
#5632=CYLINDRICAL_SURFACE('',#6588,0.25175);
#5633=CYLINDRICAL_SURFACE('',#6589,0.25175);
#5634=CYLINDRICAL_SURFACE('',#6590,0.25175);
#5635=CYLINDRICAL_SURFACE('',#6591,0.25175);
#5636=CYLINDRICAL_SURFACE('',#6593,0.25175);
#5637=CYLINDRICAL_SURFACE('',#6595,0.25175);
#5638=CYLINDRICAL_SURFACE('',#6596,0.25175);
#5639=CYLINDRICAL_SURFACE('',#6597,0.25175);
#5640=CYLINDRICAL_SURFACE('',#6598,0.25175);
#5641=CYLINDRICAL_SURFACE('',#6599,0.25175);
#5642=CYLINDRICAL_SURFACE('',#6600,0.25175);
#5643=CYLINDRICAL_SURFACE('',#6601,0.25175);
#5644=CYLINDRICAL_SURFACE('',#6603,0.30735);
#5645=CYLINDRICAL_SURFACE('',#6605,0.30735);
#5646=CYLINDRICAL_SURFACE('',#6606,0.30735);
#5647=CYLINDRICAL_SURFACE('',#6607,0.30735);
#5648=CYLINDRICAL_SURFACE('',#6608,0.30735);
#5649=CYLINDRICAL_SURFACE('',#6609,0.30735);
#5650=CYLINDRICAL_SURFACE('',#6610,0.30735);
#5651=CYLINDRICAL_SURFACE('',#6611,0.30735);
#5652=CYLINDRICAL_SURFACE('',#6613,0.30735);
#5653=CYLINDRICAL_SURFACE('',#6615,0.30735);
#5654=CYLINDRICAL_SURFACE('',#6616,0.30735);
#5655=CYLINDRICAL_SURFACE('',#6617,0.30735);
#5656=CYLINDRICAL_SURFACE('',#6618,0.30735);
#5657=CYLINDRICAL_SURFACE('',#6619,0.30735);
#5658=CYLINDRICAL_SURFACE('',#6620,0.30735);
#5659=CYLINDRICAL_SURFACE('',#6621,0.30735);
#5660=CYLINDRICAL_SURFACE('',#6623,0.30735);
#5661=CYLINDRICAL_SURFACE('',#6625,0.30735);
#5662=CYLINDRICAL_SURFACE('',#6626,0.30735);
#5663=CYLINDRICAL_SURFACE('',#6627,0.30735);
#5664=CYLINDRICAL_SURFACE('',#6628,0.30735);
#5665=CYLINDRICAL_SURFACE('',#6629,0.30735);
#5666=CYLINDRICAL_SURFACE('',#6630,0.30735);
#5667=CYLINDRICAL_SURFACE('',#6631,0.30735);
#5668=CYLINDRICAL_SURFACE('',#6633,0.30735);
#5669=CYLINDRICAL_SURFACE('',#6635,0.30735);
#5670=CYLINDRICAL_SURFACE('',#6636,0.30735);
#5671=CYLINDRICAL_SURFACE('',#6637,0.30735);
#5672=CYLINDRICAL_SURFACE('',#6638,0.30735);
#5673=CYLINDRICAL_SURFACE('',#6639,0.30735);
#5674=CYLINDRICAL_SURFACE('',#6640,0.30735);
#5675=CYLINDRICAL_SURFACE('',#6641,0.30735);
#5676=CYLINDRICAL_SURFACE('',#6643,6.35);
#5677=CYLINDRICAL_SURFACE('',#6646,6.85);
#5678=CYLINDRICAL_SURFACE('',#6659,0.30735);
#5679=CYLINDRICAL_SURFACE('',#6663,0.30735);
#5680=CYLINDRICAL_SURFACE('',#6664,0.30735);
#5681=CYLINDRICAL_SURFACE('',#6665,0.30735);
#5682=CYLINDRICAL_SURFACE('',#6666,0.25175);
#5683=CYLINDRICAL_SURFACE('',#6667,0.25175);
#5684=CYLINDRICAL_SURFACE('',#6668,0.25175);
#5685=CYLINDRICAL_SURFACE('',#6669,0.25175);
#5686=CYLINDRICAL_SURFACE('',#6670,0.35);
#5687=CYLINDRICAL_SURFACE('',#6673,0.35);
#5688=CYLINDRICAL_SURFACE('',#6676,0.35);
#5689=CYLINDRICAL_SURFACE('',#6679,0.35);
#5690=CYLINDRICAL_SURFACE('',#6685,4.8);
#5691=CYLINDRICAL_SURFACE('',#6689,3.5);
#5692=CYLINDRICAL_SURFACE('',#6694,2.7);
#5693=CYLINDRICAL_SURFACE('',#6703,2.1);
#5694=CYLINDRICAL_SURFACE('',#6704,2.1);
#5695=CYLINDRICAL_SURFACE('',#6705,1.7);
#5696=CYLINDRICAL_SURFACE('',#6706,2.1);
#5697=CYLINDRICAL_SURFACE('',#6711,8.2);
#5698=CYLINDRICAL_SURFACE('',#6723,0.35);
#5699=CYLINDRICAL_SURFACE('',#6725,0.35);
#5700=CYLINDRICAL_SURFACE('',#6727,0.35);
#5701=CYLINDRICAL_SURFACE('',#6729,0.35);
#5702=CYLINDRICAL_SURFACE('',#6734,3.);
#5703=CYLINDRICAL_SURFACE('',#6738,1.);
#5704=CYLINDRICAL_SURFACE('',#6739,1.8);
#5705=CYLINDRICAL_SURFACE('',#6740,1.8);
#5706=CYLINDRICAL_SURFACE('',#6741,6.2);
#5707=CYLINDRICAL_SURFACE('',#6745,8.2);
#5708=CYLINDRICAL_SURFACE('',#6748,0.35);
#5709=CYLINDRICAL_SURFACE('',#6751,0.35);
#5710=CYLINDRICAL_SURFACE('',#6754,0.35);
#5711=CYLINDRICAL_SURFACE('',#6757,0.35);
#5712=CYLINDRICAL_SURFACE('',#6760,1.7);
#5713=CYLINDRICAL_SURFACE('',#6768,1.1);
#5714=CYLINDRICAL_SURFACE('',#6770,2.1);
#5715=CYLINDRICAL_SURFACE('',#6774,1.7);
#5716=CYLINDRICAL_SURFACE('',#6779,0.3);
#5717=CYLINDRICAL_SURFACE('',#6781,0.3);
#5718=CYLINDRICAL_SURFACE('',#6784,0.3);
#5719=CYLINDRICAL_SURFACE('',#6788,1.);
#5720=CYLINDRICAL_SURFACE('',#6793,0.3);
#5721=CYLINDRICAL_SURFACE('',#6796,0.3);
#5722=CYLINDRICAL_SURFACE('',#6800,0.3);
#5723=CYLINDRICAL_SURFACE('',#6803,0.3);
#5724=CYLINDRICAL_SURFACE('',#6806,0.9);
#5725=CYLINDRICAL_SURFACE('',#6818,1.4);
#5726=CYLINDRICAL_SURFACE('',#6819,1.);
#5727=CYLINDRICAL_SURFACE('',#6821,1.);
#5728=CYLINDRICAL_SURFACE('',#6825,1.);
#5729=CYLINDRICAL_SURFACE('',#6828,1.5);
#5730=CYLINDRICAL_SURFACE('',#6834,1.);
#5731=CYLINDRICAL_SURFACE('',#6837,1.5);
#5732=CYLINDRICAL_SURFACE('',#6843,1.);
#5733=CYLINDRICAL_SURFACE('',#6846,1.5);
#5734=CYLINDRICAL_SURFACE('',#6852,1.);
#5735=CYLINDRICAL_SURFACE('',#6855,1.7);
#5736=CYLINDRICAL_SURFACE('',#6862,0.3);
#5737=CYLINDRICAL_SURFACE('',#6866,0.3);
#5738=CYLINDRICAL_SURFACE('',#6872,1.);
#5739=CYLINDRICAL_SURFACE('',#6875,1.7);
#5740=CYLINDRICAL_SURFACE('',#6881,1.);
#5741=CYLINDRICAL_SURFACE('',#6884,1.5);
#5742=CYLINDRICAL_SURFACE('',#6890,1.1);
#5743=CYLINDRICAL_SURFACE('',#6893,1.7);
#5744=CYLINDRICAL_SURFACE('',#6899,1.);
#5745=CYLINDRICAL_SURFACE('',#6902,1.4);
#5746=CYLINDRICAL_SURFACE('',#6913,0.9);
#5747=CYLINDRICAL_SURFACE('',#6915,1.4);
#5748=CYLINDRICAL_SURFACE('',#6919,0.2942);
#5749=CYLINDRICAL_SURFACE('',#6923,0.2942);
#5750=CYLINDRICAL_SURFACE('',#6924,0.2942);
#5751=CYLINDRICAL_SURFACE('',#6925,0.2942);
#5752=CYLINDRICAL_SURFACE('',#6926,0.2942);
#5753=CYLINDRICAL_SURFACE('',#6927,0.2942);
#5754=CYLINDRICAL_SURFACE('',#6928,0.2942);
#5755=CYLINDRICAL_SURFACE('',#6929,0.237175);
#5756=CYLINDRICAL_SURFACE('',#6931,0.237175);
#5757=CYLINDRICAL_SURFACE('',#6932,0.237175);
#5758=CYLINDRICAL_SURFACE('',#6933,0.237175);
#5759=CYLINDRICAL_SURFACE('',#6934,0.237175);
#5760=CYLINDRICAL_SURFACE('',#6935,0.237175);
#5761=CYLINDRICAL_SURFACE('',#6936,0.237175);
#5762=CYLINDRICAL_SURFACE('',#6940,0.237175);
#5763=CYLINDRICAL_SURFACE('',#6943,0.2942);
#5764=CYLINDRICAL_SURFACE('',#6953,0.5);
#5765=ADVANCED_FACE('',(#686),#5563,.T.);
#5766=ADVANCED_FACE('',(#687),#5564,.F.);
#5767=ADVANCED_FACE('',(#688,#431),#553,.T.);
#5768=ADVANCED_FACE('',(#689,#432),#554,.T.);
#5769=ADVANCED_FACE('',(#690),#5565,.F.);
#5770=ADVANCED_FACE('',(#691),#5566,.F.);
#5771=ADVANCED_FACE('',(#692),#5567,.F.);
#5772=ADVANCED_FACE('',(#693),#5568,.F.);
#5773=ADVANCED_FACE('',(#694),#555,.T.);
#5774=ADVANCED_FACE('',(#695),#5569,.F.);
#5775=ADVANCED_FACE('',(#696),#556,.T.);
#5776=ADVANCED_FACE('',(#697),#5570,.T.);
#5777=ADVANCED_FACE('',(#698),#557,.T.);
#5778=ADVANCED_FACE('',(#699),#558,.T.);
#5779=ADVANCED_FACE('',(#700),#5571,.F.);
#5780=ADVANCED_FACE('',(#701),#559,.T.);
#5781=ADVANCED_FACE('',(#702),#5572,.T.);
#5782=ADVANCED_FACE('',(#703),#560,.T.);
#5783=ADVANCED_FACE('',(#704),#561,.T.);
#5784=ADVANCED_FACE('',(#705),#5573,.F.);
#5785=ADVANCED_FACE('',(#706),#562,.T.);
#5786=ADVANCED_FACE('',(#707),#5574,.T.);
#5787=ADVANCED_FACE('',(#708),#563,.T.);
#5788=ADVANCED_FACE('',(#709),#564,.T.);
#5789=ADVANCED_FACE('',(#710),#5575,.F.);
#5790=ADVANCED_FACE('',(#711),#565,.T.);
#5791=ADVANCED_FACE('',(#712),#5576,.T.);
#5792=ADVANCED_FACE('',(#713),#566,.T.);
#5793=ADVANCED_FACE('',(#714),#567,.T.);
#5794=ADVANCED_FACE('',(#715),#5577,.F.);
#5795=ADVANCED_FACE('',(#716),#568,.T.);
#5796=ADVANCED_FACE('',(#717),#5578,.T.);
#5797=ADVANCED_FACE('',(#718),#569,.T.);
#5798=ADVANCED_FACE('',(#719),#570,.T.);
#5799=ADVANCED_FACE('',(#720),#5579,.F.);
#5800=ADVANCED_FACE('',(#721),#571,.T.);
#5801=ADVANCED_FACE('',(#722),#5580,.T.);
#5802=ADVANCED_FACE('',(#723),#572,.T.);
#5803=ADVANCED_FACE('',(#724),#573,.T.);
#5804=ADVANCED_FACE('',(#725),#574,.T.);
#5805=ADVANCED_FACE('',(#726),#575,.T.);
#5806=ADVANCED_FACE('',(#727),#576,.T.);
#5807=ADVANCED_FACE('',(#728,#433),#577,.F.);
#5808=ADVANCED_FACE('',(#729),#5581,.T.);
#5809=ADVANCED_FACE('',(#730),#5582,.T.);
#5810=ADVANCED_FACE('',(#731),#5583,.T.);
#5811=ADVANCED_FACE('',(#732),#5584,.F.);
#5812=ADVANCED_FACE('',(#733,#434,#435,#436,#437,#438,#439,#440),#578,.T.);
#5813=ADVANCED_FACE('',(#734),#579,.T.);
#5814=ADVANCED_FACE('',(#735),#580,.T.);
#5815=ADVANCED_FACE('',(#736,#441,#442,#443),#5585,.F.);
#5816=ADVANCED_FACE('',(#737),#5586,.T.);
#5817=ADVANCED_FACE('',(#738,#444,#445,#446,#447,#448),#581,.T.);
#5818=ADVANCED_FACE('',(#739,#449,#450,#451,#452,#453),#582,.F.);
#5819=ADVANCED_FACE('',(#740),#5587,.T.);
#5820=ADVANCED_FACE('',(#741),#5588,.F.);
#5821=ADVANCED_FACE('',(#742,#454),#583,.T.);
#5822=ADVANCED_FACE('',(#743,#455),#584,.T.);
#5823=ADVANCED_FACE('',(#744),#5589,.F.);
#5824=ADVANCED_FACE('',(#745),#5590,.F.);
#5825=ADVANCED_FACE('',(#746),#5591,.F.);
#5826=ADVANCED_FACE('',(#747),#5592,.F.);
#5827=ADVANCED_FACE('',(#748),#5593,.F.);
#5828=ADVANCED_FACE('',(#749),#5594,.T.);
#5829=ADVANCED_FACE('',(#750,#456,#457,#458,#459,#460),#585,.T.);
#5830=ADVANCED_FACE('',(#751,#461,#462,#463,#464,#465),#586,.F.);
#5831=ADVANCED_FACE('',(#752),#587,.F.);
#5832=ADVANCED_FACE('',(#753),#588,.F.);
#5833=ADVANCED_FACE('',(#754),#589,.F.);
#5834=ADVANCED_FACE('',(#755),#590,.F.);
#5835=ADVANCED_FACE('',(#756,#466,#467,#468,#469,#470,#471,#472),#591,.F.);
#5836=ADVANCED_FACE('',(#757),#5595,.F.);
#5837=ADVANCED_FACE('',(#758),#592,.T.);
#5838=ADVANCED_FACE('',(#759),#5596,.T.);
#5839=ADVANCED_FACE('',(#760),#593,.T.);
#5840=ADVANCED_FACE('',(#761),#594,.F.);
#5841=ADVANCED_FACE('',(#762),#5597,.F.);
#5842=ADVANCED_FACE('',(#763),#595,.T.);
#5843=ADVANCED_FACE('',(#764),#5598,.T.);
#5844=ADVANCED_FACE('',(#765),#596,.T.);
#5845=ADVANCED_FACE('',(#766),#597,.F.);
#5846=ADVANCED_FACE('',(#767),#5599,.F.);
#5847=ADVANCED_FACE('',(#768),#598,.T.);
#5848=ADVANCED_FACE('',(#769),#5600,.T.);
#5849=ADVANCED_FACE('',(#770),#599,.T.);
#5850=ADVANCED_FACE('',(#771),#600,.F.);
#5851=ADVANCED_FACE('',(#772),#5601,.F.);
#5852=ADVANCED_FACE('',(#773),#601,.T.);
#5853=ADVANCED_FACE('',(#774),#5602,.T.);
#5854=ADVANCED_FACE('',(#775),#602,.T.);
#5855=ADVANCED_FACE('',(#776),#603,.F.);
#5856=ADVANCED_FACE('',(#777),#5603,.F.);
#5857=ADVANCED_FACE('',(#778),#604,.T.);
#5858=ADVANCED_FACE('',(#779),#5604,.T.);
#5859=ADVANCED_FACE('',(#780),#605,.T.);
#5860=ADVANCED_FACE('',(#781),#606,.F.);
#5861=ADVANCED_FACE('',(#782),#5605,.F.);
#5862=ADVANCED_FACE('',(#783),#607,.T.);
#5863=ADVANCED_FACE('',(#784),#5606,.T.);
#5864=ADVANCED_FACE('',(#785),#608,.T.);
#5865=ADVANCED_FACE('',(#786),#609,.F.);
#5866=ADVANCED_FACE('',(#787),#5607,.T.);
#5867=ADVANCED_FACE('',(#788,#473),#610,.T.);
#5868=ADVANCED_FACE('',(#789),#5608,.F.);
#5869=ADVANCED_FACE('',(#790),#5609,.T.);
#5870=ADVANCED_FACE('',(#791,#474),#611,.T.);
#5871=ADVANCED_FACE('',(#792),#5610,.F.);
#5872=ADVANCED_FACE('',(#793),#5611,.T.);
#5873=ADVANCED_FACE('',(#794,#475),#612,.T.);
#5874=ADVANCED_FACE('',(#795,#476),#613,.F.);
#5875=ADVANCED_FACE('',(#796),#5612,.F.);
#5876=ADVANCED_FACE('',(#797),#5613,.F.);
#5877=ADVANCED_FACE('',(#798),#5614,.F.);
#5878=ADVANCED_FACE('',(#799),#5615,.F.);
#5879=ADVANCED_FACE('',(#800),#5616,.F.);
#5880=ADVANCED_FACE('',(#801),#5617,.F.);
#5881=ADVANCED_FACE('',(#802),#5618,.F.);
#5882=ADVANCED_FACE('',(#803),#5619,.F.);
#5883=ADVANCED_FACE('',(#804),#5620,.F.);
#5884=ADVANCED_FACE('',(#805),#5621,.F.);
#5885=ADVANCED_FACE('',(#806),#5622,.F.);
#5886=ADVANCED_FACE('',(#807),#5623,.F.);
#5887=ADVANCED_FACE('',(#808),#5624,.F.);
#5888=ADVANCED_FACE('',(#809),#5625,.F.);
#5889=ADVANCED_FACE('',(#810),#5626,.F.);
#5890=ADVANCED_FACE('',(#811),#5627,.F.);
#5891=ADVANCED_FACE('',(#812),#5628,.F.);
#5892=ADVANCED_FACE('',(#813),#5629,.F.);
#5893=ADVANCED_FACE('',(#814),#5630,.F.);
#5894=ADVANCED_FACE('',(#815),#5631,.F.);
#5895=ADVANCED_FACE('',(#816),#5632,.F.);
#5896=ADVANCED_FACE('',(#817),#5633,.F.);
#5897=ADVANCED_FACE('',(#818),#5634,.F.);
#5898=ADVANCED_FACE('',(#819),#5635,.F.);
#5899=ADVANCED_FACE('',(#820),#5636,.F.);
#5900=ADVANCED_FACE('',(#821),#5637,.F.);
#5901=ADVANCED_FACE('',(#822),#5638,.F.);
#5902=ADVANCED_FACE('',(#823),#5639,.F.);
#5903=ADVANCED_FACE('',(#824),#5640,.F.);
#5904=ADVANCED_FACE('',(#825),#5641,.F.);
#5905=ADVANCED_FACE('',(#826),#5642,.F.);
#5906=ADVANCED_FACE('',(#827),#5643,.F.);
#5907=ADVANCED_FACE('',(#828),#5644,.F.);
#5908=ADVANCED_FACE('',(#829),#5645,.F.);
#5909=ADVANCED_FACE('',(#830),#5646,.F.);
#5910=ADVANCED_FACE('',(#831),#5647,.F.);
#5911=ADVANCED_FACE('',(#832),#5648,.F.);
#5912=ADVANCED_FACE('',(#833),#5649,.F.);
#5913=ADVANCED_FACE('',(#834),#5650,.F.);
#5914=ADVANCED_FACE('',(#835),#5651,.F.);
#5915=ADVANCED_FACE('',(#836),#5652,.F.);
#5916=ADVANCED_FACE('',(#837),#5653,.F.);
#5917=ADVANCED_FACE('',(#838),#5654,.F.);
#5918=ADVANCED_FACE('',(#839),#5655,.F.);
#5919=ADVANCED_FACE('',(#840),#5656,.F.);
#5920=ADVANCED_FACE('',(#841),#5657,.F.);
#5921=ADVANCED_FACE('',(#842),#5658,.F.);
#5922=ADVANCED_FACE('',(#843),#5659,.F.);
#5923=ADVANCED_FACE('',(#844),#5660,.F.);
#5924=ADVANCED_FACE('',(#845),#5661,.F.);
#5925=ADVANCED_FACE('',(#846),#5662,.F.);
#5926=ADVANCED_FACE('',(#847),#5663,.F.);
#5927=ADVANCED_FACE('',(#848),#5664,.F.);
#5928=ADVANCED_FACE('',(#849),#5665,.F.);
#5929=ADVANCED_FACE('',(#850),#5666,.F.);
#5930=ADVANCED_FACE('',(#851),#5667,.F.);
#5931=ADVANCED_FACE('',(#852),#5668,.F.);
#5932=ADVANCED_FACE('',(#853),#5669,.F.);
#5933=ADVANCED_FACE('',(#854),#5670,.F.);
#5934=ADVANCED_FACE('',(#855),#5671,.F.);
#5935=ADVANCED_FACE('',(#856),#5672,.F.);
#5936=ADVANCED_FACE('',(#857),#5673,.F.);
#5937=ADVANCED_FACE('',(#858),#5674,.F.);
#5938=ADVANCED_FACE('',(#859),#5675,.F.);
#5939=ADVANCED_FACE('',(#860),#5676,.T.);
#5940=ADVANCED_FACE('',(#861),#5677,.F.);
#5941=ADVANCED_FACE('',(#862,#477),#614,.T.);
#5942=ADVANCED_FACE('',(#863,#478,#479,#480,#481),#615,.T.);
#5943=ADVANCED_FACE('',(#864),#5678,.F.);
#5944=ADVANCED_FACE('',(#865),#138,.F.);
#5945=ADVANCED_FACE('',(#866),#139,.F.);
#5946=ADVANCED_FACE('',(#867,#482,#483,#484,#485,#486),#616,.F.);
#5947=ADVANCED_FACE('',(#868),#5679,.F.);
#5948=ADVANCED_FACE('',(#869),#140,.F.);
#5949=ADVANCED_FACE('',(#870),#141,.F.);
#5950=ADVANCED_FACE('',(#871),#5680,.F.);
#5951=ADVANCED_FACE('',(#872),#142,.F.);
#5952=ADVANCED_FACE('',(#873),#143,.F.);
#5953=ADVANCED_FACE('',(#874),#5681,.F.);
#5954=ADVANCED_FACE('',(#875),#144,.F.);
#5955=ADVANCED_FACE('',(#876),#145,.F.);
#5956=ADVANCED_FACE('',(#877),#5682,.F.);
#5957=ADVANCED_FACE('',(#878),#5683,.F.);
#5958=ADVANCED_FACE('',(#879),#5684,.F.);
#5959=ADVANCED_FACE('',(#880),#5685,.F.);
#5960=ADVANCED_FACE('',(#881),#5686,.F.);
#5961=ADVANCED_FACE('',(#882),#5687,.F.);
#5962=ADVANCED_FACE('',(#883),#5688,.F.);
#5963=ADVANCED_FACE('',(#884),#5689,.F.);
#5964=ADVANCED_FACE('',(#885,#487,#488,#489,#490,#491),#617,.T.);
#5965=ADVANCED_FACE('',(#886),#5690,.T.);
#5966=ADVANCED_FACE('',(#887,#492,#493,#494,#495,#496),#618,.F.);
#5967=ADVANCED_FACE('',(#888),#5691,.T.);
#5968=ADVANCED_FACE('',(#889),#619,.T.);
#5969=ADVANCED_FACE('',(#890),#620,.T.);
#5970=ADVANCED_FACE('',(#891),#621,.T.);
#5971=ADVANCED_FACE('',(#892),#622,.T.);
#5972=ADVANCED_FACE('',(#893),#5692,.F.);
#5973=ADVANCED_FACE('',(#894,#497),#623,.F.);
#5974=ADVANCED_FACE('',(#895),#5693,.T.);
#5975=ADVANCED_FACE('',(#896),#5694,.T.);
#5976=ADVANCED_FACE('',(#897),#5695,.F.);
#5977=ADVANCED_FACE('',(#898),#5696,.T.);
#5978=ADVANCED_FACE('',(#899),#624,.T.);
#5979=ADVANCED_FACE('',(#900,#498,#499,#500,#501,#502),#625,.T.);
#5980=ADVANCED_FACE('',(#901),#626,.T.);
#5981=ADVANCED_FACE('',(#902),#5697,.T.);
#5982=ADVANCED_FACE('',(#903),#137,.T.);
#5983=ADVANCED_FACE('',(#904,#503,#504,#505,#506,#507),#627,.T.);
#5984=ADVANCED_FACE('',(#905),#5698,.F.);
#5985=ADVANCED_FACE('',(#906),#5699,.F.);
#5986=ADVANCED_FACE('',(#907),#5700,.F.);
#5987=ADVANCED_FACE('',(#908),#5701,.F.);
#5988=ADVANCED_FACE('',(#909,#508,#509,#510,#511,#512),#628,.F.);
#5989=ADVANCED_FACE('',(#910),#5702,.T.);
#5990=ADVANCED_FACE('',(#911,#513),#629,.F.);
#5991=ADVANCED_FACE('',(#912),#5703,.F.);
#5992=ADVANCED_FACE('',(#913),#5704,.T.);
#5993=ADVANCED_FACE('',(#914),#5705,.T.);
#5994=ADVANCED_FACE('',(#915),#5706,.F.);
#5995=ADVANCED_FACE('',(#916,#514),#5707,.T.);
#5996=ADVANCED_FACE('',(#917),#5708,.F.);
#5997=ADVANCED_FACE('',(#918),#5709,.F.);
#5998=ADVANCED_FACE('',(#919),#5710,.F.);
#5999=ADVANCED_FACE('',(#920),#5711,.F.);
#6000=ADVANCED_FACE('',(#921),#5712,.F.);
#6001=ADVANCED_FACE('',(#922,#515),#630,.F.);
#6002=ADVANCED_FACE('',(#923,#516),#631,.T.);
#6003=ADVANCED_FACE('',(#924),#5713,.F.);
#6004=ADVANCED_FACE('',(#925),#5714,.T.);
#6005=ADVANCED_FACE('',(#926,#517),#632,.F.);
#6006=ADVANCED_FACE('',(#927,#518),#633,.F.);
#6007=ADVANCED_FACE('',(#928),#5715,.F.);
#6008=ADVANCED_FACE('',(#929,#519,#520,#521,#522,#523),#634,.T.);
#6009=ADVANCED_FACE('',(#930,#524,#525,#526,#527,#528),#635,.F.);
#6010=ADVANCED_FACE('',(#931),#5716,.F.);
#6011=ADVANCED_FACE('',(#932),#5717,.F.);
#6012=ADVANCED_FACE('',(#933),#636,.F.);
#6013=ADVANCED_FACE('',(#934),#5718,.F.);
#6014=ADVANCED_FACE('',(#935),#637,.F.);
#6015=ADVANCED_FACE('',(#936),#638,.T.);
#6016=ADVANCED_FACE('',(#937),#5719,.T.);
#6017=ADVANCED_FACE('',(#938),#639,.F.);
#6018=ADVANCED_FACE('',(#939),#5720,.F.);
#6019=ADVANCED_FACE('',(#940),#640,.F.);
#6020=ADVANCED_FACE('',(#941),#5721,.F.);
#6021=ADVANCED_FACE('',(#942),#641,.T.);
#6022=ADVANCED_FACE('',(#943),#642,.F.);
#6023=ADVANCED_FACE('',(#944),#5722,.F.);
#6024=ADVANCED_FACE('',(#945),#643,.F.);
#6025=ADVANCED_FACE('',(#946),#5723,.F.);
#6026=ADVANCED_FACE('',(#947),#644,.T.);
#6027=ADVANCED_FACE('',(#948),#5724,.T.);
#6028=ADVANCED_FACE('',(#949,#529),#645,.F.);
#6029=ADVANCED_FACE('',(#950,#530),#646,.F.);
#6030=ADVANCED_FACE('',(#951,#531),#647,.T.);
#6031=ADVANCED_FACE('',(#952,#532),#648,.F.);
#6032=ADVANCED_FACE('',(#953),#5725,.T.);
#6033=ADVANCED_FACE('',(#954),#5726,.T.);
#6034=ADVANCED_FACE('',(#955,#533,#534),#5727,.T.);
#6035=ADVANCED_FACE('',(#956),#649,.T.);
#6036=ADVANCED_FACE('',(#957),#650,.F.);
#6037=ADVANCED_FACE('',(#958),#5728,.F.);
#6038=ADVANCED_FACE('',(#959),#5729,.T.);
#6039=ADVANCED_FACE('',(#960,#535),#651,.T.);
#6040=ADVANCED_FACE('',(#961,#536),#652,.F.);
#6041=ADVANCED_FACE('',(#962),#5730,.F.);
#6042=ADVANCED_FACE('',(#963),#5731,.T.);
#6043=ADVANCED_FACE('',(#964,#537),#653,.T.);
#6044=ADVANCED_FACE('',(#965,#538),#654,.F.);
#6045=ADVANCED_FACE('',(#966),#5732,.F.);
#6046=ADVANCED_FACE('',(#967),#5733,.T.);
#6047=ADVANCED_FACE('',(#968,#539),#655,.T.);
#6048=ADVANCED_FACE('',(#969,#540),#656,.F.);
#6049=ADVANCED_FACE('',(#970),#5734,.F.);
#6050=ADVANCED_FACE('',(#971),#5735,.T.);
#6051=ADVANCED_FACE('',(#972,#541),#657,.T.);
#6052=ADVANCED_FACE('',(#973,#542),#658,.F.);
#6053=ADVANCED_FACE('',(#974),#659,.T.);
#6054=ADVANCED_FACE('',(#975),#5736,.T.);
#6055=ADVANCED_FACE('',(#976),#660,.T.);
#6056=ADVANCED_FACE('',(#977),#5737,.T.);
#6057=ADVANCED_FACE('',(#978),#661,.T.);
#6058=ADVANCED_FACE('',(#979),#662,.F.);
#6059=ADVANCED_FACE('',(#980),#5738,.F.);
#6060=ADVANCED_FACE('',(#981),#5739,.T.);
#6061=ADVANCED_FACE('',(#982,#543),#663,.T.);
#6062=ADVANCED_FACE('',(#983,#544),#664,.F.);
#6063=ADVANCED_FACE('',(#984),#5740,.F.);
#6064=ADVANCED_FACE('',(#985),#5741,.T.);
#6065=ADVANCED_FACE('',(#986,#545),#665,.T.);
#6066=ADVANCED_FACE('',(#987,#546),#666,.F.);
#6067=ADVANCED_FACE('',(#988),#5742,.F.);
#6068=ADVANCED_FACE('',(#989),#5743,.T.);
#6069=ADVANCED_FACE('',(#990,#547),#667,.T.);
#6070=ADVANCED_FACE('',(#991,#548),#668,.F.);
#6071=ADVANCED_FACE('',(#992),#5744,.F.);
#6072=ADVANCED_FACE('',(#993),#5745,.T.);
#6073=ADVANCED_FACE('',(#994,#549),#669,.T.);
#6074=ADVANCED_FACE('',(#995,#550),#670,.F.);
#6075=ADVANCED_FACE('',(#996),#671,.F.);
#6076=ADVANCED_FACE('',(#997),#672,.F.);
#6077=ADVANCED_FACE('',(#998),#673,.F.);
#6078=ADVANCED_FACE('',(#999),#5746,.F.);
#6079=ADVANCED_FACE('',(#1000),#5747,.T.);
#6080=ADVANCED_FACE('',(#1001),#674,.T.);
#6081=ADVANCED_FACE('',(#1002),#5748,.T.);
#6082=ADVANCED_FACE('',(#1003),#5749,.T.);
#6083=ADVANCED_FACE('',(#1004),#5750,.T.);
#6084=ADVANCED_FACE('',(#1005),#5751,.T.);
#6085=ADVANCED_FACE('',(#1006),#5752,.T.);
#6086=ADVANCED_FACE('',(#1007),#5753,.T.);
#6087=ADVANCED_FACE('',(#1008),#5754,.T.);
#6088=ADVANCED_FACE('',(#1009),#5755,.T.);
#6089=ADVANCED_FACE('',(#1010),#5756,.T.);
#6090=ADVANCED_FACE('',(#1011),#5757,.T.);
#6091=ADVANCED_FACE('',(#1012),#5758,.T.);
#6092=ADVANCED_FACE('',(#1013),#5759,.T.);
#6093=ADVANCED_FACE('',(#1014),#5760,.T.);
#6094=ADVANCED_FACE('',(#1015),#5761,.T.);
#6095=ADVANCED_FACE('',(#1016),#135,.T.);
#6096=ADVANCED_FACE('',(#1017),#146,.F.);
#6097=ADVANCED_FACE('',(#1018),#5762,.T.);
#6098=ADVANCED_FACE('',(#1019),#147,.F.);
#6099=ADVANCED_FACE('',(#1020),#675,.T.);
#6100=ADVANCED_FACE('',(#1021),#5763,.T.);
#6101=ADVANCED_FACE('',(#1022),#676,.F.);
#6102=ADVANCED_FACE('',(#1023),#677,.F.);
#6103=ADVANCED_FACE('',(#1024),#678,.F.);
#6104=ADVANCED_FACE('',(#1025),#679,.F.);
#6105=ADVANCED_FACE('',(#1026),#680,.F.);
#6106=ADVANCED_FACE('',(#1027),#681,.F.);
#6107=ADVANCED_FACE('',(#1028),#682,.F.);
#6108=ADVANCED_FACE('',(#1029,#551),#683,.T.);
#6109=ADVANCED_FACE('',(#1030),#5764,.T.);
#6110=ADVANCED_FACE('',(#1031,#552),#684,.F.);
#6111=ADVANCED_FACE('',(#1032),#685,.T.);
#6112=CLOSED_SHELL('',(#5765,#5766,#5767,#5768,#5769,#5770,#5771,#5772,
#5773,#5774,#5775,#5776,#5777,#5778,#5779,#5780,#5781,#5782,#5783,#5784,
#5785,#5786,#5787,#5788,#5789,#5790,#5791,#5792,#5793,#5794,#5795,#5796,
#5797,#5798,#5799,#5800,#5801,#5802,#5803,#5804,#5805,#5806,#5807,#5808,
#5809,#5810,#5811,#5812,#5813,#5814,#5815,#5816,#5817,#5818));
#6113=CLOSED_SHELL('',(#5819,#5820,#5821,#5822,#5823,#5824,#5825,#5826,
#5827,#5828,#5829,#5830));
#6114=CLOSED_SHELL('',(#5831,#5832,#5833,#5834,#5835,#5836,#5837,#5838,
#5839,#5840,#5841,#5842,#5843,#5844,#5845,#5846,#5847,#5848,#5849,#5850,
#5851,#5852,#5853,#5854,#5855,#5856,#5857,#5858,#5859,#5860,#5861,#5862,
#5863,#5864,#5865,#5866,#5867,#5868,#5869,#5870));
#6115=CLOSED_SHELL('',(#5871,#5872,#5873,#5874));
#6116=CLOSED_SHELL('',(#5875,#5876,#5877,#5878,#5879,#5880,#5881,#5882,
#5883,#5884,#5885,#5886,#5887,#5888,#5889,#5890,#5891,#5892,#5893,#5894,
#5895,#5896,#5897,#5898,#5899,#5900,#5901,#5902,#5903,#5904,#5905,#5906,
#5907,#5908,#5909,#5910,#5911,#5912,#5913,#5914,#5915,#5916,#5917,#5918,
#5919,#5920,#5921,#5922,#5923,#5924,#5925,#5926,#5927,#5928,#5929,#5930,
#5931,#5932,#5933,#5934,#5935,#5936,#5937,#5938,#5939,#5940,#5941,#5942,
#5943,#5944,#5945,#5946,#5947,#5948,#5949,#5950,#5951,#5952,#5953,#5954,
#5955,#5956,#5957,#5958,#5959,#5960,#5961,#5962,#5963,#5964,#5965,#5966,
#5967,#5968,#5969,#5970,#5971,#5972,#5973,#5974,#5975,#5976,#5977,#5978,
#5979,#5980,#5981));
#6117=CLOSED_SHELL('',(#5982));
#6118=CLOSED_SHELL('',(#5983,#5984,#5985,#5986,#5987,#5988,#5989,#5990,
#5991,#5992,#5993,#5994,#5995,#5996,#5997,#5998,#5999,#6000,#6001,#6002,
#6003,#6004,#6005,#6006,#6007,#6008,#6009));
#6119=CLOSED_SHELL('',(#6010,#6011,#6012,#6013,#6014,#6015,#6016,#6017,
#6018,#6019,#6020,#6021,#6022,#6023,#6024,#6025,#6026,#6027,#6028,#6029,
#6030,#6031,#6032,#6033,#6034,#6035,#6036));
#6120=CLOSED_SHELL('',(#6037,#6038,#6039,#6040));
#6121=CLOSED_SHELL('',(#6041,#6042,#6043,#6044));
#6122=CLOSED_SHELL('',(#6045,#6046,#6047,#6048));
#6123=CLOSED_SHELL('',(#6049,#6050,#6051,#6052));
#6124=CLOSED_SHELL('',(#6053,#6054,#6055,#6056,#6057,#6058));
#6125=CLOSED_SHELL('',(#6059,#6060,#6061,#6062));
#6126=CLOSED_SHELL('',(#6063,#6064,#6065,#6066));
#6127=CLOSED_SHELL('',(#6067,#6068,#6069,#6070));
#6128=CLOSED_SHELL('',(#6071,#6072,#6073,#6074));
#6129=CLOSED_SHELL('',(#6075,#6076,#6077,#6078,#6079,#6080));
#6130=CLOSED_SHELL('',(#6081,#6082,#6083,#6084,#6085,#6086,#6087,#6088,
#6089,#6090,#6091,#6092,#6093,#6094,#6095,#6096,#6097,#6098,#6099,#6100,
#6101,#6102,#6103,#6104,#6105,#6106,#6107,#6108,#6109,#6110,#6111));
#6131=DERIVED_UNIT_ELEMENT(#6169,1.);
#6132=DERIVED_UNIT_ELEMENT(#16689,-3.);
#6133=DERIVED_UNIT_ELEMENT(#6169,1.);
#6134=DERIVED_UNIT_ELEMENT(#16689,-3.);
#6135=DERIVED_UNIT_ELEMENT(#6169,1.);
#6136=DERIVED_UNIT_ELEMENT(#16689,-3.);
#6137=DERIVED_UNIT_ELEMENT(#6169,1.);
#6138=DERIVED_UNIT_ELEMENT(#16689,-3.);
#6139=DERIVED_UNIT_ELEMENT(#6169,1.);
#6140=DERIVED_UNIT_ELEMENT(#16689,-3.);
#6141=DERIVED_UNIT_ELEMENT(#6169,1.);
#6142=DERIVED_UNIT_ELEMENT(#16689,-3.);
#6143=DERIVED_UNIT_ELEMENT(#6169,1.);
#6144=DERIVED_UNIT_ELEMENT(#16689,-3.);
#6145=DERIVED_UNIT_ELEMENT(#6169,1.);
#6146=DERIVED_UNIT_ELEMENT(#16689,-3.);
#6147=DERIVED_UNIT_ELEMENT(#6169,1.);
#6148=DERIVED_UNIT_ELEMENT(#16689,-3.);
#6149=DERIVED_UNIT_ELEMENT(#6169,1.);
#6150=DERIVED_UNIT_ELEMENT(#16689,-3.);
#6151=DERIVED_UNIT_ELEMENT(#6169,1.);
#6152=DERIVED_UNIT_ELEMENT(#16689,-3.);
#6153=DERIVED_UNIT_ELEMENT(#6169,1.);
#6154=DERIVED_UNIT_ELEMENT(#16689,-3.);
#6155=DERIVED_UNIT_ELEMENT(#6169,1.);
#6156=DERIVED_UNIT_ELEMENT(#16689,-3.);
#6157=DERIVED_UNIT_ELEMENT(#6169,1.);
#6158=DERIVED_UNIT_ELEMENT(#16689,-3.);
#6159=DERIVED_UNIT_ELEMENT(#6169,1.);
#6160=DERIVED_UNIT_ELEMENT(#16689,-3.);
#6161=DERIVED_UNIT_ELEMENT(#6169,1.);
#6162=DERIVED_UNIT_ELEMENT(#16689,-3.);
#6163=DERIVED_UNIT_ELEMENT(#6169,1.);
#6164=DERIVED_UNIT_ELEMENT(#16689,-3.);
#6165=DERIVED_UNIT_ELEMENT(#6169,1.);
#6166=DERIVED_UNIT_ELEMENT(#16689,-3.);
#6167=DERIVED_UNIT_ELEMENT(#6169,1.);
#6168=DERIVED_UNIT_ELEMENT(#16689,-3.);
#6169=(
MASS_UNIT()
NAMED_UNIT(*)
SI_UNIT(.KILO.,.GRAM.)
);
#6170=DERIVED_UNIT((#6131,#6132));
#6171=DERIVED_UNIT((#6133,#6134));
#6172=DERIVED_UNIT((#6135,#6136));
#6173=DERIVED_UNIT((#6137,#6138));
#6174=DERIVED_UNIT((#6139,#6140));
#6175=DERIVED_UNIT((#6141,#6142));
#6176=DERIVED_UNIT((#6143,#6144));
#6177=DERIVED_UNIT((#6145,#6146));
#6178=DERIVED_UNIT((#6147,#6148));
#6179=DERIVED_UNIT((#6149,#6150));
#6180=DERIVED_UNIT((#6151,#6152));
#6181=DERIVED_UNIT((#6153,#6154));
#6182=DERIVED_UNIT((#6155,#6156));
#6183=DERIVED_UNIT((#6157,#6158));
#6184=DERIVED_UNIT((#6159,#6160));
#6185=DERIVED_UNIT((#6161,#6162));
#6186=DERIVED_UNIT((#6163,#6164));
#6187=DERIVED_UNIT((#6165,#6166));
#6188=DERIVED_UNIT((#6167,#6168));
#6189=MEASURE_REPRESENTATION_ITEM('density measure',
POSITIVE_RATIO_MEASURE(7850.),#6170);
#6190=MEASURE_REPRESENTATION_ITEM('density measure',
POSITIVE_RATIO_MEASURE(7850.),#6171);
#6191=MEASURE_REPRESENTATION_ITEM('density measure',
POSITIVE_RATIO_MEASURE(7850.),#6172);
#6192=MEASURE_REPRESENTATION_ITEM('density measure',
POSITIVE_RATIO_MEASURE(8920.),#6173);
#6193=MEASURE_REPRESENTATION_ITEM('density measure',
POSITIVE_RATIO_MEASURE(7850.),#6174);
#6194=MEASURE_REPRESENTATION_ITEM('density measure',
POSITIVE_RATIO_MEASURE(1200.),#6175);
#6195=MEASURE_REPRESENTATION_ITEM('density measure',
POSITIVE_RATIO_MEASURE(7850.),#6176);
#6196=MEASURE_REPRESENTATION_ITEM('density measure',
POSITIVE_RATIO_MEASURE(7850.),#6177);
#6197=MEASURE_REPRESENTATION_ITEM('density measure',
POSITIVE_RATIO_MEASURE(7850.),#6178);
#6198=MEASURE_REPRESENTATION_ITEM('density measure',
POSITIVE_RATIO_MEASURE(7850.),#6179);
#6199=MEASURE_REPRESENTATION_ITEM('density measure',
POSITIVE_RATIO_MEASURE(7850.),#6180);
#6200=MEASURE_REPRESENTATION_ITEM('density measure',
POSITIVE_RATIO_MEASURE(8920.),#6181);
#6201=MEASURE_REPRESENTATION_ITEM('density measure',
POSITIVE_RATIO_MEASURE(7850.),#6182);
#6202=MEASURE_REPRESENTATION_ITEM('density measure',
POSITIVE_RATIO_MEASURE(8920.),#6183);
#6203=MEASURE_REPRESENTATION_ITEM('density measure',
POSITIVE_RATIO_MEASURE(7850.),#6184);
#6204=MEASURE_REPRESENTATION_ITEM('density measure',
POSITIVE_RATIO_MEASURE(7850.),#6185);
#6205=MEASURE_REPRESENTATION_ITEM('density measure',
POSITIVE_RATIO_MEASURE(7850.),#6186);
#6206=MEASURE_REPRESENTATION_ITEM('density measure',
POSITIVE_RATIO_MEASURE(7850.),#6187);
#6207=MEASURE_REPRESENTATION_ITEM('density measure',
POSITIVE_RATIO_MEASURE(7850.),#6188);
#6208=PROPERTY_DEFINITION_REPRESENTATION(#6303,#6246);
#6209=PROPERTY_DEFINITION_REPRESENTATION(#6304,#6247);
#6210=PROPERTY_DEFINITION_REPRESENTATION(#6305,#6248);
#6211=PROPERTY_DEFINITION_REPRESENTATION(#6306,#6249);
#6212=PROPERTY_DEFINITION_REPRESENTATION(#6307,#6250);
#6213=PROPERTY_DEFINITION_REPRESENTATION(#6308,#6251);
#6214=PROPERTY_DEFINITION_REPRESENTATION(#6309,#6252);
#6215=PROPERTY_DEFINITION_REPRESENTATION(#6310,#6253);
#6216=PROPERTY_DEFINITION_REPRESENTATION(#6311,#6254);
#6217=PROPERTY_DEFINITION_REPRESENTATION(#6312,#6255);
#6218=PROPERTY_DEFINITION_REPRESENTATION(#6313,#6256);
#6219=PROPERTY_DEFINITION_REPRESENTATION(#6314,#6257);
#6220=PROPERTY_DEFINITION_REPRESENTATION(#6315,#6258);
#6221=PROPERTY_DEFINITION_REPRESENTATION(#6316,#6259);
#6222=PROPERTY_DEFINITION_REPRESENTATION(#6317,#6260);
#6223=PROPERTY_DEFINITION_REPRESENTATION(#6318,#6261);
#6224=PROPERTY_DEFINITION_REPRESENTATION(#6319,#6262);
#6225=PROPERTY_DEFINITION_REPRESENTATION(#6320,#6263);
#6226=PROPERTY_DEFINITION_REPRESENTATION(#6321,#6264);
#6227=PROPERTY_DEFINITION_REPRESENTATION(#6322,#6265);
#6228=PROPERTY_DEFINITION_REPRESENTATION(#6323,#6266);
#6229=PROPERTY_DEFINITION_REPRESENTATION(#6324,#6267);
#6230=PROPERTY_DEFINITION_REPRESENTATION(#6325,#6268);
#6231=PROPERTY_DEFINITION_REPRESENTATION(#6326,#6269);
#6232=PROPERTY_DEFINITION_REPRESENTATION(#6327,#6270);
#6233=PROPERTY_DEFINITION_REPRESENTATION(#6328,#6271);
#6234=PROPERTY_DEFINITION_REPRESENTATION(#6329,#6272);
#6235=PROPERTY_DEFINITION_REPRESENTATION(#6330,#6273);
#6236=PROPERTY_DEFINITION_REPRESENTATION(#6331,#6274);
#6237=PROPERTY_DEFINITION_REPRESENTATION(#6332,#6275);
#6238=PROPERTY_DEFINITION_REPRESENTATION(#6333,#6276);
#6239=PROPERTY_DEFINITION_REPRESENTATION(#6334,#6277);
#6240=PROPERTY_DEFINITION_REPRESENTATION(#6335,#6278);
#6241=PROPERTY_DEFINITION_REPRESENTATION(#6336,#6279);
#6242=PROPERTY_DEFINITION_REPRESENTATION(#6337,#6280);
#6243=PROPERTY_DEFINITION_REPRESENTATION(#6338,#6281);
#6244=PROPERTY_DEFINITION_REPRESENTATION(#6339,#6282);
#6245=PROPERTY_DEFINITION_REPRESENTATION(#6340,#6283);
#6246=REPRESENTATION('material name',(#6284),#16668);
#6247=REPRESENTATION('density',(#6189),#16668);
#6248=REPRESENTATION('material name',(#6285),#16669);
#6249=REPRESENTATION('density',(#6190),#16669);
#6250=REPRESENTATION('material name',(#6286),#16670);
#6251=REPRESENTATION('density',(#6191),#16670);
#6252=REPRESENTATION('material name',(#6287),#16671);
#6253=REPRESENTATION('density',(#6192),#16671);
#6254=REPRESENTATION('material name',(#6288),#16672);
#6255=REPRESENTATION('density',(#6193),#16672);
#6256=REPRESENTATION('material name',(#6289),#16673);
#6257=REPRESENTATION('density',(#6194),#16673);
#6258=REPRESENTATION('material name',(#6290),#16674);
#6259=REPRESENTATION('density',(#6195),#16674);
#6260=REPRESENTATION('material name',(#6291),#16675);
#6261=REPRESENTATION('density',(#6196),#16675);
#6262=REPRESENTATION('material name',(#6292),#16676);
#6263=REPRESENTATION('density',(#6197),#16676);
#6264=REPRESENTATION('material name',(#6293),#16677);
#6265=REPRESENTATION('density',(#6198),#16677);
#6266=REPRESENTATION('material name',(#6294),#16678);
#6267=REPRESENTATION('density',(#6199),#16678);
#6268=REPRESENTATION('material name',(#6295),#16679);
#6269=REPRESENTATION('density',(#6200),#16679);
#6270=REPRESENTATION('material name',(#6296),#16680);
#6271=REPRESENTATION('density',(#6201),#16680);
#6272=REPRESENTATION('material name',(#6297),#16681);
#6273=REPRESENTATION('density',(#6202),#16681);
#6274=REPRESENTATION('material name',(#6298),#16682);
#6275=REPRESENTATION('density',(#6203),#16682);
#6276=REPRESENTATION('material name',(#6299),#16683);
#6277=REPRESENTATION('density',(#6204),#16683);
#6278=REPRESENTATION('material name',(#6300),#16684);
#6279=REPRESENTATION('density',(#6205),#16684);
#6280=REPRESENTATION('material name',(#6301),#16685);
#6281=REPRESENTATION('density',(#6206),#16685);
#6282=REPRESENTATION('material name',(#6302),#16686);
#6283=REPRESENTATION('density',(#6207),#16686);
#6284=DESCRIPTIVE_REPRESENTATION_ITEM('Steel','Steel');
#6285=DESCRIPTIVE_REPRESENTATION_ITEM('Steel','Steel');
#6286=DESCRIPTIVE_REPRESENTATION_ITEM('Steel','Steel');
#6287=DESCRIPTIVE_REPRESENTATION_ITEM('Copper, Alloy','Copper, Alloy');
#6288=DESCRIPTIVE_REPRESENTATION_ITEM('Steel','Steel');
#6289=DESCRIPTIVE_REPRESENTATION_ITEM('Rubber, Nitrile',
'Rubber, Nitrile');
#6290=DESCRIPTIVE_REPRESENTATION_ITEM('Steel','Steel');
#6291=DESCRIPTIVE_REPRESENTATION_ITEM('Steel','Steel');
#6292=DESCRIPTIVE_REPRESENTATION_ITEM('Steel','Steel');
#6293=DESCRIPTIVE_REPRESENTATION_ITEM('Steel','Steel');
#6294=DESCRIPTIVE_REPRESENTATION_ITEM('Steel','Steel');
#6295=DESCRIPTIVE_REPRESENTATION_ITEM('Copper, Alloy','Copper, Alloy');
#6296=DESCRIPTIVE_REPRESENTATION_ITEM('Steel','Steel');
#6297=DESCRIPTIVE_REPRESENTATION_ITEM('Copper, Alloy','Copper, Alloy');
#6298=DESCRIPTIVE_REPRESENTATION_ITEM('Steel','Steel');
#6299=DESCRIPTIVE_REPRESENTATION_ITEM('Steel','Steel');
#6300=DESCRIPTIVE_REPRESENTATION_ITEM('Steel','Steel');
#6301=DESCRIPTIVE_REPRESENTATION_ITEM('Steel','Steel');
#6302=DESCRIPTIVE_REPRESENTATION_ITEM('Steel','Steel');
#6303=PROPERTY_DEFINITION('material property','material name',#16785);
#6304=PROPERTY_DEFINITION('material property','density of part',#16785);
#6305=PROPERTY_DEFINITION('material property','material name',#16786);
#6306=PROPERTY_DEFINITION('material property','density of part',#16786);
#6307=PROPERTY_DEFINITION('material property','material name',#16787);
#6308=PROPERTY_DEFINITION('material property','density of part',#16787);
#6309=PROPERTY_DEFINITION('material property','material name',#16788);
#6310=PROPERTY_DEFINITION('material property','density of part',#16788);
#6311=PROPERTY_DEFINITION('material property','material name',#16789);
#6312=PROPERTY_DEFINITION('material property','density of part',#16789);
#6313=PROPERTY_DEFINITION('material property','material name',#16790);
#6314=PROPERTY_DEFINITION('material property','density of part',#16790);
#6315=PROPERTY_DEFINITION('material property','material name',#16791);
#6316=PROPERTY_DEFINITION('material property','density of part',#16791);
#6317=PROPERTY_DEFINITION('material property','material name',#16792);
#6318=PROPERTY_DEFINITION('material property','density of part',#16792);
#6319=PROPERTY_DEFINITION('material property','material name',#16793);
#6320=PROPERTY_DEFINITION('material property','density of part',#16793);
#6321=PROPERTY_DEFINITION('material property','material name',#16794);
#6322=PROPERTY_DEFINITION('material property','density of part',#16794);
#6323=PROPERTY_DEFINITION('material property','material name',#16795);
#6324=PROPERTY_DEFINITION('material property','density of part',#16795);
#6325=PROPERTY_DEFINITION('material property','material name',#16796);
#6326=PROPERTY_DEFINITION('material property','density of part',#16796);
#6327=PROPERTY_DEFINITION('material property','material name',#16797);
#6328=PROPERTY_DEFINITION('material property','density of part',#16797);
#6329=PROPERTY_DEFINITION('material property','material name',#16798);
#6330=PROPERTY_DEFINITION('material property','density of part',#16798);
#6331=PROPERTY_DEFINITION('material property','material name',#16799);
#6332=PROPERTY_DEFINITION('material property','density of part',#16799);
#6333=PROPERTY_DEFINITION('material property','material name',#16800);
#6334=PROPERTY_DEFINITION('material property','density of part',#16800);
#6335=PROPERTY_DEFINITION('material property','material name',#16801);
#6336=PROPERTY_DEFINITION('material property','density of part',#16801);
#6337=PROPERTY_DEFINITION('material property','material name',#16802);
#6338=PROPERTY_DEFINITION('material property','density of part',#16802);
#6339=PROPERTY_DEFINITION('material property','material name',#16803);
#6340=PROPERTY_DEFINITION('material property','density of part',#16803);
#6341=AXIS2_PLACEMENT_3D('',#8651,#6988,#6989);
#6342=AXIS2_PLACEMENT_3D('',#8652,#6990,#6991);
#6343=AXIS2_PLACEMENT_3D('',#8653,#6992,#6993);
#6344=AXIS2_PLACEMENT_3D('',#8655,#6994,#6995);
#6345=AXIS2_PLACEMENT_3D('',#8658,#6997,#6998);
#6346=AXIS2_PLACEMENT_3D('',#8659,#6999,#7000);
#6347=AXIS2_PLACEMENT_3D('',#8661,#7001,#7002);
#6348=AXIS2_PLACEMENT_3D('',#8664,#7004,#7005);
#6349=AXIS2_PLACEMENT_3D('',#8665,#7006,#7007);
#6350=AXIS2_PLACEMENT_3D('',#8666,#7008,#7009);
#6351=AXIS2_PLACEMENT_3D('',#8668,#7010,#7011);
#6352=AXIS2_PLACEMENT_3D('',#8669,#7012,#7013);
#6353=AXIS2_PLACEMENT_3D('',#8671,#7014,#7015);
#6354=AXIS2_PLACEMENT_3D('',#8674,#7017,#7018);
#6355=AXIS2_PLACEMENT_3D('',#8675,#7019,#7020);
#6356=AXIS2_PLACEMENT_3D('',#8677,#7021,#7022);
#6357=AXIS2_PLACEMENT_3D('',#8680,#7024,#7025);
#6358=AXIS2_PLACEMENT_3D('',#8681,#7026,#7027);
#6359=AXIS2_PLACEMENT_3D('',#8683,#7028,#7029);
#6360=AXIS2_PLACEMENT_3D('',#8686,#7031,#7032);
#6361=AXIS2_PLACEMENT_3D('',#8687,#7033,#7034);
#6362=AXIS2_PLACEMENT_3D('',#8689,#7035,#7036);
#6363=AXIS2_PLACEMENT_3D('',#8692,#7038,#7039);
#6364=AXIS2_PLACEMENT_3D('',#8693,#7040,#7041);
#6365=AXIS2_PLACEMENT_3D('',#8702,#7046,#7047);
#6366=AXIS2_PLACEMENT_3D('',#8704,#7048,#7049);
#6367=AXIS2_PLACEMENT_3D('',#8706,#7050,#7051);
#6368=AXIS2_PLACEMENT_3D('',#8708,#7053,#7054);
#6369=AXIS2_PLACEMENT_3D('',#8714,#7058,#7059);
#6370=AXIS2_PLACEMENT_3D('',#8715,#7060,#7061);
#6371=AXIS2_PLACEMENT_3D('',#8716,#7062,#7063);
#6372=AXIS2_PLACEMENT_3D('',#8717,#7064,#7065);
#6373=AXIS2_PLACEMENT_3D('',#8718,#7066,#7067);
#6374=AXIS2_PLACEMENT_3D('',#8727,#7072,#7073);
#6375=AXIS2_PLACEMENT_3D('',#8729,#7074,#7075);
#6376=AXIS2_PLACEMENT_3D('',#8731,#7076,#7077);
#6377=AXIS2_PLACEMENT_3D('',#8733,#7079,#7080);
#6378=AXIS2_PLACEMENT_3D('',#8739,#7084,#7085);
#6379=AXIS2_PLACEMENT_3D('',#8740,#7086,#7087);
#6380=AXIS2_PLACEMENT_3D('',#8741,#7088,#7089);
#6381=AXIS2_PLACEMENT_3D('',#8742,#7090,#7091);
#6382=AXIS2_PLACEMENT_3D('',#8743,#7092,#7093);
#6383=AXIS2_PLACEMENT_3D('',#8752,#7098,#7099);
#6384=AXIS2_PLACEMENT_3D('',#8754,#7100,#7101);
#6385=AXIS2_PLACEMENT_3D('',#8756,#7102,#7103);
#6386=AXIS2_PLACEMENT_3D('',#8758,#7105,#7106);
#6387=AXIS2_PLACEMENT_3D('',#8764,#7110,#7111);
#6388=AXIS2_PLACEMENT_3D('',#8765,#7112,#7113);
#6389=AXIS2_PLACEMENT_3D('',#8766,#7114,#7115);
#6390=AXIS2_PLACEMENT_3D('',#8767,#7116,#7117);
#6391=AXIS2_PLACEMENT_3D('',#8768,#7118,#7119);
#6392=AXIS2_PLACEMENT_3D('',#8777,#7124,#7125);
#6393=AXIS2_PLACEMENT_3D('',#8779,#7126,#7127);
#6394=AXIS2_PLACEMENT_3D('',#8781,#7128,#7129);
#6395=AXIS2_PLACEMENT_3D('',#8783,#7131,#7132);
#6396=AXIS2_PLACEMENT_3D('',#8789,#7136,#7137);
#6397=AXIS2_PLACEMENT_3D('',#8790,#7138,#7139);
#6398=AXIS2_PLACEMENT_3D('',#8791,#7140,#7141);
#6399=AXIS2_PLACEMENT_3D('',#8792,#7142,#7143);
#6400=AXIS2_PLACEMENT_3D('',#8793,#7144,#7145);
#6401=AXIS2_PLACEMENT_3D('',#8802,#7150,#7151);
#6402=AXIS2_PLACEMENT_3D('',#8804,#7152,#7153);
#6403=AXIS2_PLACEMENT_3D('',#8806,#7154,#7155);
#6404=AXIS2_PLACEMENT_3D('',#8808,#7157,#7158);
#6405=AXIS2_PLACEMENT_3D('',#8814,#7162,#7163);
#6406=AXIS2_PLACEMENT_3D('',#8815,#7164,#7165);
#6407=AXIS2_PLACEMENT_3D('',#8816,#7166,#7167);
#6408=AXIS2_PLACEMENT_3D('',#8817,#7168,#7169);
#6409=AXIS2_PLACEMENT_3D('',#8818,#7170,#7171);
#6410=AXIS2_PLACEMENT_3D('',#8827,#7176,#7177);
#6411=AXIS2_PLACEMENT_3D('',#8829,#7178,#7179);
#6412=AXIS2_PLACEMENT_3D('',#8831,#7180,#7181);
#6413=AXIS2_PLACEMENT_3D('',#8833,#7183,#7184);
#6414=AXIS2_PLACEMENT_3D('',#8839,#7188,#7189);
#6415=AXIS2_PLACEMENT_3D('',#8840,#7190,#7191);
#6416=AXIS2_PLACEMENT_3D('',#8841,#7192,#7193);
#6417=AXIS2_PLACEMENT_3D('',#8842,#7194,#7195);
#6418=AXIS2_PLACEMENT_3D('',#8843,#7196,#7197);
#6419=AXIS2_PLACEMENT_3D('',#8852,#7202,#7203);
#6420=AXIS2_PLACEMENT_3D('',#8861,#7208,#7209);
#6421=AXIS2_PLACEMENT_3D('',#8870,#7214,#7215);
#6422=AXIS2_PLACEMENT_3D('',#8879,#7220,#7221);
#6423=AXIS2_PLACEMENT_3D('',#8880,#7222,#7223);
#6424=AXIS2_PLACEMENT_3D('',#8881,#7224,#7225);
#6425=AXIS2_PLACEMENT_3D('',#8883,#7226,#7227);
#6426=AXIS2_PLACEMENT_3D('',#8887,#7229,#7230);
#6427=AXIS2_PLACEMENT_3D('',#8890,#7232,#7233);
#6428=AXIS2_PLACEMENT_3D('',#8891,#7234,#7235);
#6429=AXIS2_PLACEMENT_3D('',#8893,#7236,#7237);
#6430=AXIS2_PLACEMENT_3D('',#8894,#7238,#7239);
#6431=AXIS2_PLACEMENT_3D('',#8896,#7240,#7241);
#6432=AXIS2_PLACEMENT_3D('',#8898,#7243,#7244);
#6433=AXIS2_PLACEMENT_3D('',#8899,#7245,#7246);
#6434=AXIS2_PLACEMENT_3D('',#8900,#7247,#7248);
#6435=AXIS2_PLACEMENT_3D('',#8903,#7250,#7251);
#6436=AXIS2_PLACEMENT_3D('',#8904,#7252,#7253);
#6437=AXIS2_PLACEMENT_3D('',#8906,#7254,#7255);
#6438=AXIS2_PLACEMENT_3D('',#8908,#7257,#7258);
#6439=AXIS2_PLACEMENT_3D('',#8912,#7260,#7261);
#6440=AXIS2_PLACEMENT_3D('',#8914,#7263,#7264);
#6441=AXIS2_PLACEMENT_3D('',#8915,#7265,#7266);
#6442=AXIS2_PLACEMENT_3D('',#8916,#7267,#7268);
#6443=AXIS2_PLACEMENT_3D('',#8918,#7270,#7271);
#6444=AXIS2_PLACEMENT_3D('',#8920,#7273,#7274);
#6445=AXIS2_PLACEMENT_3D('',#8923,#7276,#7277);
#6446=AXIS2_PLACEMENT_3D('',#8924,#7278,#7279);
#6447=AXIS2_PLACEMENT_3D('',#8926,#7280,#7281);
#6448=AXIS2_PLACEMENT_3D('',#8929,#7283,#7284);
#6449=AXIS2_PLACEMENT_3D('',#8930,#7285,#7286);
#6450=AXIS2_PLACEMENT_3D('',#8931,#7287,#7288);
#6451=AXIS2_PLACEMENT_3D('',#8932,#7289,#7290);
#6452=AXIS2_PLACEMENT_3D('',#8933,#7291,#7292);
#6453=AXIS2_PLACEMENT_3D('',#8935,#7293,#7294);
#6454=AXIS2_PLACEMENT_3D('',#8938,#7296,#7297);
#6455=AXIS2_PLACEMENT_3D('',#8939,#7298,#7299);
#6456=AXIS2_PLACEMENT_3D('',#8941,#7300,#7301);
#6457=AXIS2_PLACEMENT_3D('',#8944,#7303,#7304);
#6458=AXIS2_PLACEMENT_3D('',#8945,#7305,#7306);
#6459=AXIS2_PLACEMENT_3D('',#8946,#7307,#7308);
#6460=AXIS2_PLACEMENT_3D('',#8948,#7309,#7310);
#6461=AXIS2_PLACEMENT_3D('',#8949,#7311,#7312);
#6462=AXIS2_PLACEMENT_3D('',#8951,#7313,#7314);
#6463=AXIS2_PLACEMENT_3D('',#8954,#7316,#7317);
#6464=AXIS2_PLACEMENT_3D('',#8955,#7318,#7319);
#6465=AXIS2_PLACEMENT_3D('',#8957,#7320,#7321);
#6466=AXIS2_PLACEMENT_3D('',#8960,#7323,#7324);
#6467=AXIS2_PLACEMENT_3D('',#8961,#7325,#7326);
#6468=AXIS2_PLACEMENT_3D('',#8963,#7327,#7328);
#6469=AXIS2_PLACEMENT_3D('',#8966,#7330,#7331);
#6470=AXIS2_PLACEMENT_3D('',#8967,#7332,#7333);
#6471=AXIS2_PLACEMENT_3D('',#8969,#7334,#7335);
#6472=AXIS2_PLACEMENT_3D('',#8972,#7337,#7338);
#6473=AXIS2_PLACEMENT_3D('',#8973,#7339,#7340);
#6474=AXIS2_PLACEMENT_3D('',#8976,#7342,#7343);
#6475=AXIS2_PLACEMENT_3D('',#8977,#7344,#7345);
#6476=AXIS2_PLACEMENT_3D('',#8979,#7346,#7347);
#6477=AXIS2_PLACEMENT_3D('',#8982,#7349,#7350);
#6478=AXIS2_PLACEMENT_3D('',#8983,#7351,#7352);
#6479=AXIS2_PLACEMENT_3D('',#8984,#7353,#7354);
#6480=AXIS2_PLACEMENT_3D('',#8985,#7355,#7356);
#6481=AXIS2_PLACEMENT_3D('',#8986,#7357,#7358);
#6482=AXIS2_PLACEMENT_3D('',#8995,#7363,#7364);
#6483=AXIS2_PLACEMENT_3D('',#9001,#7368,#7369);
#6484=AXIS2_PLACEMENT_3D('',#9007,#7373,#7374);
#6485=AXIS2_PLACEMENT_3D('',#9008,#7375,#7376);
#6486=AXIS2_PLACEMENT_3D('',#9009,#7377,#7378);
#6487=AXIS2_PLACEMENT_3D('',#9011,#7379,#7380);
#6488=AXIS2_PLACEMENT_3D('',#9014,#7381,#7382);
#6489=AXIS2_PLACEMENT_3D('',#9018,#7384,#7385);
#6490=AXIS2_PLACEMENT_3D('',#9022,#7387,#7388);
#6491=AXIS2_PLACEMENT_3D('',#9026,#7390,#7391);
#6492=AXIS2_PLACEMENT_3D('',#9030,#7393,#7394);
#6493=AXIS2_PLACEMENT_3D('',#9034,#7396,#7397);
#6494=AXIS2_PLACEMENT_3D('',#9038,#7399,#7400);
#6495=AXIS2_PLACEMENT_3D('',#9042,#7402,#7403);
#6496=AXIS2_PLACEMENT_3D('',#9046,#7405,#7406);
#6497=AXIS2_PLACEMENT_3D('',#9050,#7408,#7409);
#6498=AXIS2_PLACEMENT_3D('',#9054,#7411,#7412);
#6499=AXIS2_PLACEMENT_3D('',#9058,#7414,#7415);
#6500=AXIS2_PLACEMENT_3D('',#9061,#7417,#7418);
#6501=AXIS2_PLACEMENT_3D('',#9062,#7419,#7420);
#6502=AXIS2_PLACEMENT_3D('',#9063,#7421,#7422);
#6503=AXIS2_PLACEMENT_3D('',#9066,#7423,#7424);
#6504=AXIS2_PLACEMENT_3D('',#9069,#7427,#7428);
#6505=AXIS2_PLACEMENT_3D('',#9073,#7431,#7432);
#6506=AXIS2_PLACEMENT_3D('',#9075,#7433,#7434);
#6507=AXIS2_PLACEMENT_3D('',#9077,#7436,#7437);
#6508=AXIS2_PLACEMENT_3D('',#9079,#7439,#7440);
#6509=AXIS2_PLACEMENT_3D('',#9080,#7441,#7442);
#6510=AXIS2_PLACEMENT_3D('',#9083,#7443,#7444);
#6511=AXIS2_PLACEMENT_3D('',#9086,#7447,#7448);
#6512=AXIS2_PLACEMENT_3D('',#9090,#7451,#7452);
#6513=AXIS2_PLACEMENT_3D('',#9092,#7453,#7454);
#6514=AXIS2_PLACEMENT_3D('',#9094,#7456,#7457);
#6515=AXIS2_PLACEMENT_3D('',#9096,#7459,#7460);
#6516=AXIS2_PLACEMENT_3D('',#9097,#7461,#7462);
#6517=AXIS2_PLACEMENT_3D('',#9100,#7463,#7464);
#6518=AXIS2_PLACEMENT_3D('',#9103,#7467,#7468);
#6519=AXIS2_PLACEMENT_3D('',#9107,#7471,#7472);
#6520=AXIS2_PLACEMENT_3D('',#9109,#7473,#7474);
#6521=AXIS2_PLACEMENT_3D('',#9111,#7476,#7477);
#6522=AXIS2_PLACEMENT_3D('',#9113,#7479,#7480);
#6523=AXIS2_PLACEMENT_3D('',#9114,#7481,#7482);
#6524=AXIS2_PLACEMENT_3D('',#9117,#7483,#7484);
#6525=AXIS2_PLACEMENT_3D('',#9120,#7487,#7488);
#6526=AXIS2_PLACEMENT_3D('',#9124,#7491,#7492);
#6527=AXIS2_PLACEMENT_3D('',#9126,#7493,#7494);
#6528=AXIS2_PLACEMENT_3D('',#9128,#7496,#7497);
#6529=AXIS2_PLACEMENT_3D('',#9130,#7499,#7500);
#6530=AXIS2_PLACEMENT_3D('',#9131,#7501,#7502);
#6531=AXIS2_PLACEMENT_3D('',#9134,#7503,#7504);
#6532=AXIS2_PLACEMENT_3D('',#9137,#7507,#7508);
#6533=AXIS2_PLACEMENT_3D('',#9141,#7511,#7512);
#6534=AXIS2_PLACEMENT_3D('',#9143,#7513,#7514);
#6535=AXIS2_PLACEMENT_3D('',#9145,#7516,#7517);
#6536=AXIS2_PLACEMENT_3D('',#9147,#7519,#7520);
#6537=AXIS2_PLACEMENT_3D('',#9148,#7521,#7522);
#6538=AXIS2_PLACEMENT_3D('',#9151,#7523,#7524);
#6539=AXIS2_PLACEMENT_3D('',#9154,#7527,#7528);
#6540=AXIS2_PLACEMENT_3D('',#9158,#7531,#7532);
#6541=AXIS2_PLACEMENT_3D('',#9160,#7533,#7534);
#6542=AXIS2_PLACEMENT_3D('',#9162,#7536,#7537);
#6543=AXIS2_PLACEMENT_3D('',#9164,#7539,#7540);
#6544=AXIS2_PLACEMENT_3D('',#9165,#7541,#7542);
#6545=AXIS2_PLACEMENT_3D('',#9167,#7543,#7544);
#6546=AXIS2_PLACEMENT_3D('',#9170,#7546,#7547);
#6547=AXIS2_PLACEMENT_3D('',#9171,#7548,#7549);
#6548=AXIS2_PLACEMENT_3D('',#9173,#7550,#7551);
#6549=AXIS2_PLACEMENT_3D('',#9174,#7552,#7553);
#6550=AXIS2_PLACEMENT_3D('',#9176,#7555,#7556);
#6551=AXIS2_PLACEMENT_3D('',#9178,#7557,#7558);
#6552=AXIS2_PLACEMENT_3D('',#9180,#7560,#7561);
#6553=AXIS2_PLACEMENT_3D('',#9181,#7562,#7563);
#6554=AXIS2_PLACEMENT_3D('',#9182,#7564,#7565);
#6555=AXIS2_PLACEMENT_3D('',#9184,#7566,#7567);
#6556=AXIS2_PLACEMENT_3D('',#9187,#7569,#7570);
#6557=AXIS2_PLACEMENT_3D('',#9188,#7571,#7572);
#6558=AXIS2_PLACEMENT_3D('',#9190,#7573,#7574);
#6559=AXIS2_PLACEMENT_3D('',#9193,#7576,#7577);
#6560=AXIS2_PLACEMENT_3D('',#9194,#7578,#7579);
#6561=AXIS2_PLACEMENT_3D('',#9195,#7580,#7581);
#6562=AXIS2_PLACEMENT_3D('',#9196,#7582,#7583);
#6563=AXIS2_PLACEMENT_3D('',#9197,#7584,#7585);
#6564=AXIS2_PLACEMENT_3D('',#9207,#7587,#7588);
#6565=AXIS2_PLACEMENT_3D('',#9218,#7589,#7590);
#6566=AXIS2_PLACEMENT_3D('',#9269,#7592,#7593);
#6567=AXIS2_PLACEMENT_3D('',#9320,#7595,#7596);
#6568=AXIS2_PLACEMENT_3D('',#9368,#7598,#7599);
#6569=AXIS2_PLACEMENT_3D('',#9419,#7601,#7602);
#6570=AXIS2_PLACEMENT_3D('',#9470,#7604,#7605);
#6571=AXIS2_PLACEMENT_3D('',#9518,#7607,#7608);
#6572=AXIS2_PLACEMENT_3D('',#9537,#7610,#7611);
#6573=AXIS2_PLACEMENT_3D('',#9557,#7612,#7613);
#6574=AXIS2_PLACEMENT_3D('',#9567,#7615,#7616);
#6575=AXIS2_PLACEMENT_3D('',#9578,#7617,#7618);
#6576=AXIS2_PLACEMENT_3D('',#9629,#7620,#7621);
#6577=AXIS2_PLACEMENT_3D('',#9680,#7623,#7624);
#6578=AXIS2_PLACEMENT_3D('',#9728,#7626,#7627);
#6579=AXIS2_PLACEMENT_3D('',#9779,#7629,#7630);
#6580=AXIS2_PLACEMENT_3D('',#9830,#7632,#7633);
#6581=AXIS2_PLACEMENT_3D('',#9878,#7635,#7636);
#6582=AXIS2_PLACEMENT_3D('',#9897,#7638,#7639);
#6583=AXIS2_PLACEMENT_3D('',#9917,#7640,#7641);
#6584=AXIS2_PLACEMENT_3D('',#9927,#7643,#7644);
#6585=AXIS2_PLACEMENT_3D('',#9938,#7645,#7646);
#6586=AXIS2_PLACEMENT_3D('',#9989,#7648,#7649);
#6587=AXIS2_PLACEMENT_3D('',#10040,#7651,#7652);
#6588=AXIS2_PLACEMENT_3D('',#10088,#7654,#7655);
#6589=AXIS2_PLACEMENT_3D('',#10139,#7657,#7658);
#6590=AXIS2_PLACEMENT_3D('',#10190,#7660,#7661);
#6591=AXIS2_PLACEMENT_3D('',#10238,#7663,#7664);
#6592=AXIS2_PLACEMENT_3D('',#10257,#7666,#7667);
#6593=AXIS2_PLACEMENT_3D('',#10277,#7668,#7669);
#6594=AXIS2_PLACEMENT_3D('',#10287,#7671,#7672);
#6595=AXIS2_PLACEMENT_3D('',#10298,#7673,#7674);
#6596=AXIS2_PLACEMENT_3D('',#10349,#7676,#7677);
#6597=AXIS2_PLACEMENT_3D('',#10400,#7679,#7680);
#6598=AXIS2_PLACEMENT_3D('',#10448,#7682,#7683);
#6599=AXIS2_PLACEMENT_3D('',#10499,#7685,#7686);
#6600=AXIS2_PLACEMENT_3D('',#10550,#7688,#7689);
#6601=AXIS2_PLACEMENT_3D('',#10598,#7691,#7692);
#6602=AXIS2_PLACEMENT_3D('',#10617,#7694,#7695);
#6603=AXIS2_PLACEMENT_3D('',#10637,#7696,#7697);
#6604=AXIS2_PLACEMENT_3D('',#10651,#7699,#7700);
#6605=AXIS2_PLACEMENT_3D('',#10661,#7701,#7702);
#6606=AXIS2_PLACEMENT_3D('',#10685,#7704,#7705);
#6607=AXIS2_PLACEMENT_3D('',#10710,#7707,#7708);
#6608=AXIS2_PLACEMENT_3D('',#10735,#7710,#7711);
#6609=AXIS2_PLACEMENT_3D('',#10759,#7713,#7714);
#6610=AXIS2_PLACEMENT_3D('',#10784,#7716,#7717);
#6611=AXIS2_PLACEMENT_3D('',#10809,#7719,#7720);
#6612=AXIS2_PLACEMENT_3D('',#10820,#7722,#7723);
#6613=AXIS2_PLACEMENT_3D('',#10826,#7724,#7725);
#6614=AXIS2_PLACEMENT_3D('',#10840,#7727,#7728);
#6615=AXIS2_PLACEMENT_3D('',#10850,#7729,#7730);
#6616=AXIS2_PLACEMENT_3D('',#10874,#7732,#7733);
#6617=AXIS2_PLACEMENT_3D('',#10899,#7735,#7736);
#6618=AXIS2_PLACEMENT_3D('',#10924,#7738,#7739);
#6619=AXIS2_PLACEMENT_3D('',#10948,#7741,#7742);
#6620=AXIS2_PLACEMENT_3D('',#10973,#7744,#7745);
#6621=AXIS2_PLACEMENT_3D('',#10998,#7747,#7748);
#6622=AXIS2_PLACEMENT_3D('',#11009,#7750,#7751);
#6623=AXIS2_PLACEMENT_3D('',#11015,#7752,#7753);
#6624=AXIS2_PLACEMENT_3D('',#11029,#7755,#7756);
#6625=AXIS2_PLACEMENT_3D('',#11039,#7757,#7758);
#6626=AXIS2_PLACEMENT_3D('',#11063,#7760,#7761);
#6627=AXIS2_PLACEMENT_3D('',#11088,#7763,#7764);
#6628=AXIS2_PLACEMENT_3D('',#11113,#7766,#7767);
#6629=AXIS2_PLACEMENT_3D('',#11137,#7769,#7770);
#6630=AXIS2_PLACEMENT_3D('',#11162,#7772,#7773);
#6631=AXIS2_PLACEMENT_3D('',#11187,#7775,#7776);
#6632=AXIS2_PLACEMENT_3D('',#11198,#7778,#7779);
#6633=AXIS2_PLACEMENT_3D('',#11204,#7780,#7781);
#6634=AXIS2_PLACEMENT_3D('',#11218,#7783,#7784);
#6635=AXIS2_PLACEMENT_3D('',#11228,#7785,#7786);
#6636=AXIS2_PLACEMENT_3D('',#11252,#7788,#7789);
#6637=AXIS2_PLACEMENT_3D('',#11277,#7791,#7792);
#6638=AXIS2_PLACEMENT_3D('',#11302,#7794,#7795);
#6639=AXIS2_PLACEMENT_3D('',#11326,#7797,#7798);
#6640=AXIS2_PLACEMENT_3D('',#11351,#7800,#7801);
#6641=AXIS2_PLACEMENT_3D('',#11376,#7803,#7804);
#6642=AXIS2_PLACEMENT_3D('',#11387,#7806,#7807);
#6643=AXIS2_PLACEMENT_3D('',#11393,#7808,#7809);
#6644=AXIS2_PLACEMENT_3D('',#11395,#7810,#7811);
#6645=AXIS2_PLACEMENT_3D('',#11398,#7813,#7814);
#6646=AXIS2_PLACEMENT_3D('',#11399,#7815,#7816);
#6647=AXIS2_PLACEMENT_3D('',#11401,#7817,#7818);
#6648=AXIS2_PLACEMENT_3D('',#11404,#7820,#7821);
#6649=AXIS2_PLACEMENT_3D('',#11405,#7822,#7823);
#6650=AXIS2_PLACEMENT_3D('',#11406,#7824,#7825);
#6651=AXIS2_PLACEMENT_3D('',#11409,#7826,#7827);
#6652=AXIS2_PLACEMENT_3D('',#11411,#7828,#7829);
#6653=AXIS2_PLACEMENT_3D('',#11415,#7831,#7832);
#6654=AXIS2_PLACEMENT_3D('',#11419,#7834,#7835);
#6655=AXIS2_PLACEMENT_3D('',#11423,#7837,#7838);
#6656=AXIS2_PLACEMENT_3D('',#11429,#7841,#7842);
#6657=AXIS2_PLACEMENT_3D('',#11432,#7844,#7845);
#6658=AXIS2_PLACEMENT_3D('',#11434,#7846,#7847);
#6659=AXIS2_PLACEMENT_3D('',#11435,#7848,#7849);
#6660=AXIS2_PLACEMENT_3D('',#12187,#7850,#7851);
#6661=AXIS2_PLACEMENT_3D('',#12189,#7852,#7853);
#6662=AXIS2_PLACEMENT_3D('',#12191,#7854,#7855);
#6663=AXIS2_PLACEMENT_3D('',#12540,#7856,#7857);
#6664=AXIS2_PLACEMENT_3D('',#13176,#7858,#7859);
#6665=AXIS2_PLACEMENT_3D('',#13812,#7860,#7861);
#6666=AXIS2_PLACEMENT_3D('',#14448,#7862,#7863);
#6667=AXIS2_PLACEMENT_3D('',#14449,#7864,#7865);
#6668=AXIS2_PLACEMENT_3D('',#14450,#7866,#7867);
#6669=AXIS2_PLACEMENT_3D('',#14451,#7868,#7869);
#6670=AXIS2_PLACEMENT_3D('',#14452,#7870,#7871);
#6671=AXIS2_PLACEMENT_3D('',#14454,#7872,#7873);
#6672=AXIS2_PLACEMENT_3D('',#14457,#7875,#7876);
#6673=AXIS2_PLACEMENT_3D('',#14458,#7877,#7878);
#6674=AXIS2_PLACEMENT_3D('',#14460,#7879,#7880);
#6675=AXIS2_PLACEMENT_3D('',#14463,#7882,#7883);
#6676=AXIS2_PLACEMENT_3D('',#14464,#7884,#7885);
#6677=AXIS2_PLACEMENT_3D('',#14466,#7886,#7887);
#6678=AXIS2_PLACEMENT_3D('',#14469,#7889,#7890);
#6679=AXIS2_PLACEMENT_3D('',#14470,#7891,#7892);
#6680=AXIS2_PLACEMENT_3D('',#14472,#7893,#7894);
#6681=AXIS2_PLACEMENT_3D('',#14475,#7896,#7897);
#6682=AXIS2_PLACEMENT_3D('',#14476,#7898,#7899);
#6683=AXIS2_PLACEMENT_3D('',#14478,#7900,#7901);
#6684=AXIS2_PLACEMENT_3D('',#14480,#7902,#7903);
#6685=AXIS2_PLACEMENT_3D('',#14481,#7904,#7905);
#6686=AXIS2_PLACEMENT_3D('',#14484,#7907,#7908);
#6687=AXIS2_PLACEMENT_3D('',#14485,#7909,#7910);
#6688=AXIS2_PLACEMENT_3D('',#14487,#7911,#7912);
#6689=AXIS2_PLACEMENT_3D('',#14488,#7913,#7914);
#6690=AXIS2_PLACEMENT_3D('',#14490,#7916,#7917);
#6691=AXIS2_PLACEMENT_3D('',#14496,#7921,#7922);
#6692=AXIS2_PLACEMENT_3D('',#14502,#7926,#7927);
#6693=AXIS2_PLACEMENT_3D('',#14508,#7931,#7932);
#6694=AXIS2_PLACEMENT_3D('',#14514,#7936,#7937);
#6695=AXIS2_PLACEMENT_3D('',#14518,#7939,#7940);
#6696=AXIS2_PLACEMENT_3D('',#14520,#7942,#7943);
#6697=AXIS2_PLACEMENT_3D('',#14522,#7945,#7946);
#6698=AXIS2_PLACEMENT_3D('',#14523,#7947,#7948);
#6699=AXIS2_PLACEMENT_3D('',#14526,#7950,#7951);
#6700=AXIS2_PLACEMENT_3D('',#14527,#7952,#7953);
#6701=AXIS2_PLACEMENT_3D('',#14529,#7954,#7955);
#6702=AXIS2_PLACEMENT_3D('',#14532,#7957,#7958);
#6703=AXIS2_PLACEMENT_3D('',#14533,#7959,#7960);
#6704=AXIS2_PLACEMENT_3D('',#14535,#7962,#7963);
#6705=AXIS2_PLACEMENT_3D('',#14536,#7964,#7965);
#6706=AXIS2_PLACEMENT_3D('',#14538,#7967,#7968);
#6707=AXIS2_PLACEMENT_3D('',#14540,#7970,#7971);
#6708=AXIS2_PLACEMENT_3D('',#14541,#7972,#7973);
#6709=AXIS2_PLACEMENT_3D('',#14543,#7974,#7975);
#6710=AXIS2_PLACEMENT_3D('',#14544,#7976,#7977);
#6711=AXIS2_PLACEMENT_3D('',#14545,#7978,#7979);
#6712=AXIS2_PLACEMENT_3D('',#14547,#7981,#7982);
#6713=AXIS2_PLACEMENT_3D('',#14630,#7983,#7984);
#6714=AXIS2_PLACEMENT_3D('',#14631,#7985,#7986);
#6715=AXIS2_PLACEMENT_3D('',#14632,#7987,#7988);
#6716=AXIS2_PLACEMENT_3D('',#14633,#7989,#7990);
#6717=AXIS2_PLACEMENT_3D('',#14635,#7991,#7992);
#6718=AXIS2_PLACEMENT_3D('',#14637,#7993,#7994);
#6719=AXIS2_PLACEMENT_3D('',#14639,#7995,#7996);
#6720=AXIS2_PLACEMENT_3D('',#14641,#7997,#7998);
#6721=AXIS2_PLACEMENT_3D('',#14643,#7999,#8000);
#6722=AXIS2_PLACEMENT_3D('',#14645,#8001,#8002);
#6723=AXIS2_PLACEMENT_3D('',#14646,#8003,#8004);
#6724=AXIS2_PLACEMENT_3D('',#14649,#8006,#8007);
#6725=AXIS2_PLACEMENT_3D('',#14650,#8008,#8009);
#6726=AXIS2_PLACEMENT_3D('',#14653,#8011,#8012);
#6727=AXIS2_PLACEMENT_3D('',#14654,#8013,#8014);
#6728=AXIS2_PLACEMENT_3D('',#14657,#8016,#8017);
#6729=AXIS2_PLACEMENT_3D('',#14658,#8018,#8019);
#6730=AXIS2_PLACEMENT_3D('',#14661,#8021,#8022);
#6731=AXIS2_PLACEMENT_3D('',#14662,#8023,#8024);
#6732=AXIS2_PLACEMENT_3D('',#14664,#8025,#8026);
#6733=AXIS2_PLACEMENT_3D('',#14666,#8027,#8028);
#6734=AXIS2_PLACEMENT_3D('',#14667,#8029,#8030);
#6735=AXIS2_PLACEMENT_3D('',#14669,#8032,#8033);
#6736=AXIS2_PLACEMENT_3D('',#14673,#8035,#8036);
#6737=AXIS2_PLACEMENT_3D('',#14675,#8037,#8038);
#6738=AXIS2_PLACEMENT_3D('',#14676,#8039,#8040);
#6739=AXIS2_PLACEMENT_3D('',#14678,#8042,#8043);
#6740=AXIS2_PLACEMENT_3D('',#14750,#8045,#8046);
#6741=AXIS2_PLACEMENT_3D('',#14810,#8049,#8050);
#6742=AXIS2_PLACEMENT_3D('',#14812,#8051,#8052);
#6743=AXIS2_PLACEMENT_3D('',#14815,#8054,#8055);
#6744=AXIS2_PLACEMENT_3D('',#14816,#8056,#8057);
#6745=AXIS2_PLACEMENT_3D('',#14817,#8058,#8059);
#6746=AXIS2_PLACEMENT_3D('',#14819,#8060,#8061);
#6747=AXIS2_PLACEMENT_3D('',#14822,#8063,#8064);
#6748=AXIS2_PLACEMENT_3D('',#14823,#8065,#8066);
#6749=AXIS2_PLACEMENT_3D('',#14825,#8067,#8068);
#6750=AXIS2_PLACEMENT_3D('',#14828,#8070,#8071);
#6751=AXIS2_PLACEMENT_3D('',#14829,#8072,#8073);
#6752=AXIS2_PLACEMENT_3D('',#14831,#8074,#8075);
#6753=AXIS2_PLACEMENT_3D('',#14834,#8077,#8078);
#6754=AXIS2_PLACEMENT_3D('',#14835,#8079,#8080);
#6755=AXIS2_PLACEMENT_3D('',#14837,#8081,#8082);
#6756=AXIS2_PLACEMENT_3D('',#14840,#8084,#8085);
#6757=AXIS2_PLACEMENT_3D('',#14841,#8086,#8087);
#6758=AXIS2_PLACEMENT_3D('',#14843,#8088,#8089);
#6759=AXIS2_PLACEMENT_3D('',#14846,#8091,#8092);
#6760=AXIS2_PLACEMENT_3D('',#14847,#8093,#8094);
#6761=AXIS2_PLACEMENT_3D('',#14849,#8095,#8096);
#6762=AXIS2_PLACEMENT_3D('',#14852,#8098,#8099);
#6763=AXIS2_PLACEMENT_3D('',#14853,#8100,#8101);
#6764=AXIS2_PLACEMENT_3D('',#14855,#8102,#8103);
#6765=AXIS2_PLACEMENT_3D('',#14856,#8104,#8105);
#6766=AXIS2_PLACEMENT_3D('',#14858,#8106,#8107);
#6767=AXIS2_PLACEMENT_3D('',#14860,#8108,#8109);
#6768=AXIS2_PLACEMENT_3D('',#14861,#8110,#8111);
#6769=AXIS2_PLACEMENT_3D('',#14864,#8113,#8114);
#6770=AXIS2_PLACEMENT_3D('',#14865,#8115,#8116);
#6771=AXIS2_PLACEMENT_3D('',#14867,#8117,#8118);
#6772=AXIS2_PLACEMENT_3D('',#14869,#8120,#8121);
#6773=AXIS2_PLACEMENT_3D('',#14870,#8122,#8123);
#6774=AXIS2_PLACEMENT_3D('',#14871,#8124,#8125);
#6775=AXIS2_PLACEMENT_3D('',#14873,#8126,#8127);
#6776=AXIS2_PLACEMENT_3D('',#14875,#8129,#8130);
#6777=AXIS2_PLACEMENT_3D('',#14876,#8131,#8132);
#6778=AXIS2_PLACEMENT_3D('',#14877,#8133,#8134);
#6779=AXIS2_PLACEMENT_3D('',#14878,#8135,#8136);
#6780=AXIS2_PLACEMENT_3D('',#14883,#8138,#8139);
#6781=AXIS2_PLACEMENT_3D('',#14896,#8141,#8142);
#6782=AXIS2_PLACEMENT_3D('',#14910,#8144,#8145);
#6783=AXIS2_PLACEMENT_3D('',#14912,#8147,#8148);
#6784=AXIS2_PLACEMENT_3D('',#14918,#8152,#8153);
#6785=AXIS2_PLACEMENT_3D('',#14939,#8154,#8155);
#6786=AXIS2_PLACEMENT_3D('',#14941,#8157,#8158);
#6787=AXIS2_PLACEMENT_3D('',#14944,#8161,#8162);
#6788=AXIS2_PLACEMENT_3D('',#14945,#8163,#8164);
#6789=AXIS2_PLACEMENT_3D('',#14947,#8165,#8166);
#6790=AXIS2_PLACEMENT_3D('',#14948,#8167,#8168);
#6791=AXIS2_PLACEMENT_3D('',#14951,#8170,#8171);
#6792=AXIS2_PLACEMENT_3D('',#14952,#8172,#8173);
#6793=AXIS2_PLACEMENT_3D('',#14961,#8178,#8179);
#6794=AXIS2_PLACEMENT_3D('',#14982,#8180,#8181);
#6795=AXIS2_PLACEMENT_3D('',#14984,#8183,#8184);
#6796=AXIS2_PLACEMENT_3D('',#14990,#8188,#8189);
#6797=AXIS2_PLACEMENT_3D('',#15009,#8190,#8191);
#6798=AXIS2_PLACEMENT_3D('',#15010,#8192,#8193);
#6799=AXIS2_PLACEMENT_3D('',#15011,#8194,#8195);
#6800=AXIS2_PLACEMENT_3D('',#15020,#8200,#8201);
#6801=AXIS2_PLACEMENT_3D('',#15041,#8202,#8203);
#6802=AXIS2_PLACEMENT_3D('',#15043,#8205,#8206);
#6803=AXIS2_PLACEMENT_3D('',#15049,#8210,#8211);
#6804=AXIS2_PLACEMENT_3D('',#15068,#8212,#8213);
#6805=AXIS2_PLACEMENT_3D('',#15069,#8214,#8215);
#6806=AXIS2_PLACEMENT_3D('',#15070,#8216,#8217);
#6807=AXIS2_PLACEMENT_3D('',#15072,#8218,#8219);
#6808=AXIS2_PLACEMENT_3D('',#15075,#8221,#8222);
#6809=AXIS2_PLACEMENT_3D('',#15076,#8223,#8224);
#6810=AXIS2_PLACEMENT_3D('',#15078,#8225,#8226);
#6811=AXIS2_PLACEMENT_3D('',#15079,#8227,#8228);
#6812=AXIS2_PLACEMENT_3D('',#15080,#8229,#8230);
#6813=AXIS2_PLACEMENT_3D('',#15082,#8231,#8232);
#6814=AXIS2_PLACEMENT_3D('',#15084,#8233,#8234);
#6815=AXIS2_PLACEMENT_3D('',#15085,#8235,#8236);
#6816=AXIS2_PLACEMENT_3D('',#15087,#8237,#8238);
#6817=AXIS2_PLACEMENT_3D('',#15089,#8239,#8240);
#6818=AXIS2_PLACEMENT_3D('',#15090,#8241,#8242);
#6819=AXIS2_PLACEMENT_3D('',#15092,#8244,#8245);
#6820=AXIS2_PLACEMENT_3D('',#15095,#8247,#8248);
#6821=AXIS2_PLACEMENT_3D('',#15096,#8249,#8250);
#6822=AXIS2_PLACEMENT_3D('',#15098,#8252,#8253);
#6823=AXIS2_PLACEMENT_3D('',#15099,#8254,#8255);
#6824=AXIS2_PLACEMENT_3D('',#15100,#8256,#8257);
#6825=AXIS2_PLACEMENT_3D('',#15101,#8258,#8259);
#6826=AXIS2_PLACEMENT_3D('',#15103,#8260,#8261);
#6827=AXIS2_PLACEMENT_3D('',#15106,#8263,#8264);
#6828=AXIS2_PLACEMENT_3D('',#15107,#8265,#8266);
#6829=AXIS2_PLACEMENT_3D('',#15109,#8267,#8268);
#6830=AXIS2_PLACEMENT_3D('',#15112,#8270,#8271);
#6831=AXIS2_PLACEMENT_3D('',#15113,#8272,#8273);
#6832=AXIS2_PLACEMENT_3D('',#15114,#8274,#8275);
#6833=AXIS2_PLACEMENT_3D('',#15115,#8276,#8277);
#6834=AXIS2_PLACEMENT_3D('',#15116,#8278,#8279);
#6835=AXIS2_PLACEMENT_3D('',#15118,#8280,#8281);
#6836=AXIS2_PLACEMENT_3D('',#15121,#8283,#8284);
#6837=AXIS2_PLACEMENT_3D('',#15122,#8285,#8286);
#6838=AXIS2_PLACEMENT_3D('',#15124,#8287,#8288);
#6839=AXIS2_PLACEMENT_3D('',#15127,#8290,#8291);
#6840=AXIS2_PLACEMENT_3D('',#15128,#8292,#8293);
#6841=AXIS2_PLACEMENT_3D('',#15129,#8294,#8295);
#6842=AXIS2_PLACEMENT_3D('',#15130,#8296,#8297);
#6843=AXIS2_PLACEMENT_3D('',#15131,#8298,#8299);
#6844=AXIS2_PLACEMENT_3D('',#15133,#8300,#8301);
#6845=AXIS2_PLACEMENT_3D('',#15136,#8303,#8304);
#6846=AXIS2_PLACEMENT_3D('',#15137,#8305,#8306);
#6847=AXIS2_PLACEMENT_3D('',#15139,#8307,#8308);
#6848=AXIS2_PLACEMENT_3D('',#15142,#8310,#8311);
#6849=AXIS2_PLACEMENT_3D('',#15143,#8312,#8313);
#6850=AXIS2_PLACEMENT_3D('',#15144,#8314,#8315);
#6851=AXIS2_PLACEMENT_3D('',#15145,#8316,#8317);
#6852=AXIS2_PLACEMENT_3D('',#15146,#8318,#8319);
#6853=AXIS2_PLACEMENT_3D('',#15148,#8320,#8321);
#6854=AXIS2_PLACEMENT_3D('',#15151,#8323,#8324);
#6855=AXIS2_PLACEMENT_3D('',#15152,#8325,#8326);
#6856=AXIS2_PLACEMENT_3D('',#15154,#8327,#8328);
#6857=AXIS2_PLACEMENT_3D('',#15157,#8330,#8331);
#6858=AXIS2_PLACEMENT_3D('',#15158,#8332,#8333);
#6859=AXIS2_PLACEMENT_3D('',#15159,#8334,#8335);
#6860=AXIS2_PLACEMENT_3D('',#15160,#8336,#8337);
#6861=AXIS2_PLACEMENT_3D('',#15161,#8338,#8339);
#6862=AXIS2_PLACEMENT_3D('',#15170,#8344,#8345);
#6863=AXIS2_PLACEMENT_3D('',#15172,#8346,#8347);
#6864=AXIS2_PLACEMENT_3D('',#15174,#8348,#8349);
#6865=AXIS2_PLACEMENT_3D('',#15176,#8351,#8352);
#6866=AXIS2_PLACEMENT_3D('',#15182,#8356,#8357);
#6867=AXIS2_PLACEMENT_3D('',#15183,#8358,#8359);
#6868=AXIS2_PLACEMENT_3D('',#15184,#8360,#8361);
#6869=AXIS2_PLACEMENT_3D('',#15185,#8362,#8363);
#6870=AXIS2_PLACEMENT_3D('',#15186,#8364,#8365);
#6871=AXIS2_PLACEMENT_3D('',#15187,#8366,#8367);
#6872=AXIS2_PLACEMENT_3D('',#15188,#8368,#8369);
#6873=AXIS2_PLACEMENT_3D('',#15190,#8370,#8371);
#6874=AXIS2_PLACEMENT_3D('',#15193,#8373,#8374);
#6875=AXIS2_PLACEMENT_3D('',#15194,#8375,#8376);
#6876=AXIS2_PLACEMENT_3D('',#15196,#8377,#8378);
#6877=AXIS2_PLACEMENT_3D('',#15199,#8380,#8381);
#6878=AXIS2_PLACEMENT_3D('',#15200,#8382,#8383);
#6879=AXIS2_PLACEMENT_3D('',#15201,#8384,#8385);
#6880=AXIS2_PLACEMENT_3D('',#15202,#8386,#8387);
#6881=AXIS2_PLACEMENT_3D('',#15203,#8388,#8389);
#6882=AXIS2_PLACEMENT_3D('',#15205,#8390,#8391);
#6883=AXIS2_PLACEMENT_3D('',#15208,#8393,#8394);
#6884=AXIS2_PLACEMENT_3D('',#15209,#8395,#8396);
#6885=AXIS2_PLACEMENT_3D('',#15211,#8397,#8398);
#6886=AXIS2_PLACEMENT_3D('',#15214,#8400,#8401);
#6887=AXIS2_PLACEMENT_3D('',#15215,#8402,#8403);
#6888=AXIS2_PLACEMENT_3D('',#15216,#8404,#8405);
#6889=AXIS2_PLACEMENT_3D('',#15217,#8406,#8407);
#6890=AXIS2_PLACEMENT_3D('',#15218,#8408,#8409);
#6891=AXIS2_PLACEMENT_3D('',#15220,#8410,#8411);
#6892=AXIS2_PLACEMENT_3D('',#15223,#8413,#8414);
#6893=AXIS2_PLACEMENT_3D('',#15224,#8415,#8416);
#6894=AXIS2_PLACEMENT_3D('',#15226,#8417,#8418);
#6895=AXIS2_PLACEMENT_3D('',#15229,#8420,#8421);
#6896=AXIS2_PLACEMENT_3D('',#15230,#8422,#8423);
#6897=AXIS2_PLACEMENT_3D('',#15231,#8424,#8425);
#6898=AXIS2_PLACEMENT_3D('',#15232,#8426,#8427);
#6899=AXIS2_PLACEMENT_3D('',#15233,#8428,#8429);
#6900=AXIS2_PLACEMENT_3D('',#15235,#8430,#8431);
#6901=AXIS2_PLACEMENT_3D('',#15238,#8433,#8434);
#6902=AXIS2_PLACEMENT_3D('',#15239,#8435,#8436);
#6903=AXIS2_PLACEMENT_3D('',#15241,#8437,#8438);
#6904=AXIS2_PLACEMENT_3D('',#15244,#8440,#8441);
#6905=AXIS2_PLACEMENT_3D('',#15245,#8442,#8443);
#6906=AXIS2_PLACEMENT_3D('',#15246,#8444,#8445);
#6907=AXIS2_PLACEMENT_3D('',#15247,#8446,#8447);
#6908=AXIS2_PLACEMENT_3D('',#15248,#8448,#8449);
#6909=AXIS2_PLACEMENT_3D('',#15257,#8454,#8455);
#6910=AXIS2_PLACEMENT_3D('',#15266,#8460,#8461);
#6911=AXIS2_PLACEMENT_3D('',#15267,#8462,#8463);
#6912=AXIS2_PLACEMENT_3D('',#15268,#8464,#8465);
#6913=AXIS2_PLACEMENT_3D('',#15269,#8466,#8467);
#6914=AXIS2_PLACEMENT_3D('',#15270,#8468,#8469);
#6915=AXIS2_PLACEMENT_3D('',#15271,#8470,#8471);
#6916=AXIS2_PLACEMENT_3D('',#15272,#8472,#8473);
#6917=AXIS2_PLACEMENT_3D('',#15273,#8474,#8475);
#6918=AXIS2_PLACEMENT_3D('',#15274,#8476,#8477);
#6919=AXIS2_PLACEMENT_3D('',#15275,#8478,#8479);
#6920=AXIS2_PLACEMENT_3D('',#15291,#8481,#8482);
#6921=AXIS2_PLACEMENT_3D('',#15294,#8484,#8485);
#6922=AXIS2_PLACEMENT_3D('',#15296,#8486,#8487);
#6923=AXIS2_PLACEMENT_3D('',#15304,#8488,#8489);
#6924=AXIS2_PLACEMENT_3D('',#15352,#8491,#8492);
#6925=AXIS2_PLACEMENT_3D('',#15400,#8494,#8495);
#6926=AXIS2_PLACEMENT_3D('',#15448,#8497,#8498);
#6927=AXIS2_PLACEMENT_3D('',#15502,#8500,#8501);
#6928=AXIS2_PLACEMENT_3D('',#15550,#8503,#8504);
#6929=AXIS2_PLACEMENT_3D('',#15598,#8506,#8507);
#6930=AXIS2_PLACEMENT_3D('',#15614,#8509,#8510);
#6931=AXIS2_PLACEMENT_3D('',#15623,#8511,#8512);
#6932=AXIS2_PLACEMENT_3D('',#15648,#8514,#8515);
#6933=AXIS2_PLACEMENT_3D('',#15672,#8517,#8518);
#6934=AXIS2_PLACEMENT_3D('',#15697,#8520,#8521);
#6935=AXIS2_PLACEMENT_3D('',#15722,#8523,#8524);
#6936=AXIS2_PLACEMENT_3D('',#15746,#8526,#8527);
#6937=AXIS2_PLACEMENT_3D('',#15770,#8529,#8530);
#6938=AXIS2_PLACEMENT_3D('',#15953,#8531,#8532);
#6939=AXIS2_PLACEMENT_3D('',#15975,#8534,#8535);
#6940=AXIS2_PLACEMENT_3D('',#16266,#8536,#8537);
#6941=AXIS2_PLACEMENT_3D('',#16277,#8538,#8539);
#6942=AXIS2_PLACEMENT_3D('',#16567,#8540,#8541);
#6943=AXIS2_PLACEMENT_3D('',#16568,#8542,#8543);
#6944=AXIS2_PLACEMENT_3D('',#16569,#8544,#8545);
#6945=AXIS2_PLACEMENT_3D('',#16578,#8550,#8551);
#6946=AXIS2_PLACEMENT_3D('',#16584,#8555,#8556);
#6947=AXIS2_PLACEMENT_3D('',#16590,#8560,#8561);
#6948=AXIS2_PLACEMENT_3D('',#16596,#8565,#8566);
#6949=AXIS2_PLACEMENT_3D('',#16602,#8570,#8571);
#6950=AXIS2_PLACEMENT_3D('',#16605,#8574,#8575);
#6951=AXIS2_PLACEMENT_3D('',#16606,#8576,#8577);
#6952=AXIS2_PLACEMENT_3D('',#16608,#8578,#8579);
#6953=AXIS2_PLACEMENT_3D('',#16609,#8580,#8581);
#6954=AXIS2_PLACEMENT_3D('',#16612,#8583,#8584);
#6955=AXIS2_PLACEMENT_3D('',#16613,#8585,#8586);
#6956=AXIS2_PLACEMENT_3D('',#16614,#8587,#8588);
#6957=AXIS2_PLACEMENT_3D('',#16615,#8589,#8590);
#6958=AXIS2_PLACEMENT_3D('',#16616,#8591,#8592);
#6959=AXIS2_PLACEMENT_3D('',#16617,#8593,#8594);
#6960=AXIS2_PLACEMENT_3D('',#16618,#8595,#8596);
#6961=AXIS2_PLACEMENT_3D('',#16619,#8597,#8598);
#6962=AXIS2_PLACEMENT_3D('',#16620,#8599,#8600);
#6963=AXIS2_PLACEMENT_3D('',#16621,#8601,#8602);
#6964=AXIS2_PLACEMENT_3D('',#16622,#8603,#8604);
#6965=AXIS2_PLACEMENT_3D('',#16623,#8605,#8606);
#6966=AXIS2_PLACEMENT_3D('',#16624,#8607,#8608);
#6967=AXIS2_PLACEMENT_3D('',#16625,#8609,#8610);
#6968=AXIS2_PLACEMENT_3D('',#16626,#8611,#8612);
#6969=AXIS2_PLACEMENT_3D('',#16627,#8613,#8614);
#6970=AXIS2_PLACEMENT_3D('',#16628,#8615,#8616);
#6971=AXIS2_PLACEMENT_3D('',#16629,#8617,#8618);
#6972=AXIS2_PLACEMENT_3D('',#16630,#8619,#8620);
#6973=AXIS2_PLACEMENT_3D('',#16631,#8621,#8622);
#6974=AXIS2_PLACEMENT_3D('',#16632,#8623,#8624);
#6975=AXIS2_PLACEMENT_3D('',#16633,#8625,#8626);
#6976=AXIS2_PLACEMENT_3D('',#16634,#8627,#8628);
#6977=AXIS2_PLACEMENT_3D('',#16635,#8629,#8630);
#6978=AXIS2_PLACEMENT_3D('',#16636,#8631,#8632);
#6979=AXIS2_PLACEMENT_3D('',#16637,#8633,#8634);
#6980=AXIS2_PLACEMENT_3D('',#16638,#8635,#8636);
#6981=AXIS2_PLACEMENT_3D('',#16639,#8637,#8638);
#6982=AXIS2_PLACEMENT_3D('',#16640,#8639,#8640);
#6983=AXIS2_PLACEMENT_3D('',#16641,#8641,#8642);
#6984=AXIS2_PLACEMENT_3D('',#16642,#8643,#8644);
#6985=AXIS2_PLACEMENT_3D('',#16643,#8645,#8646);
#6986=AXIS2_PLACEMENT_3D('',#16644,#8647,#8648);
#6987=AXIS2_PLACEMENT_3D('',#16645,#8649,#8650);
#6988=DIRECTION('axis',(0.,0.,1.));
#6989=DIRECTION('refdir',(1.,0.,0.));
#6990=DIRECTION('axis',(0.,0.,1.));
#6991=DIRECTION('refdir',(1.,0.,0.));
#6992=DIRECTION('center_axis',(0.,0.,-1.));
#6993=DIRECTION('ref_axis',(1.,0.,0.));
#6994=DIRECTION('center_axis',(0.,0.,1.));
#6995=DIRECTION('ref_axis',(1.,0.,0.));
#6996=DIRECTION('',(0.,0.,-1.));
#6997=DIRECTION('center_axis',(0.,0.,1.));
#6998=DIRECTION('ref_axis',(1.,0.,0.));
#6999=DIRECTION('center_axis',(0.,0.,-1.));
#7000=DIRECTION('ref_axis',(1.,0.,0.));
#7001=DIRECTION('center_axis',(0.,0.,-1.));
#7002=DIRECTION('ref_axis',(1.,0.,0.));
#7003=DIRECTION('',(0.,0.,-1.));
#7004=DIRECTION('center_axis',(0.,0.,-1.));
#7005=DIRECTION('ref_axis',(1.,0.,0.));
#7006=DIRECTION('center_axis',(0.,0.,1.));
#7007=DIRECTION('ref_axis',(1.,0.,0.));
#7008=DIRECTION('center_axis',(0.,0.,1.));
#7009=DIRECTION('ref_axis',(1.,0.,0.));
#7010=DIRECTION('center_axis',(0.,0.,-1.));
#7011=DIRECTION('ref_axis',(1.,0.,0.));
#7012=DIRECTION('center_axis',(0.,0.,-1.));
#7013=DIRECTION('ref_axis',(1.,0.,0.));
#7014=DIRECTION('center_axis',(0.,0.,-1.));
#7015=DIRECTION('ref_axis',(1.,0.,0.));
#7016=DIRECTION('',(0.,0.,-1.));
#7017=DIRECTION('center_axis',(0.,0.,1.));
#7018=DIRECTION('ref_axis',(1.,0.,0.));
#7019=DIRECTION('center_axis',(0.,0.,-1.));
#7020=DIRECTION('ref_axis',(1.,0.,0.));
#7021=DIRECTION('center_axis',(0.,0.,-1.));
#7022=DIRECTION('ref_axis',(1.,0.,0.));
#7023=DIRECTION('',(0.,0.,-1.));
#7024=DIRECTION('center_axis',(0.,0.,1.));
#7025=DIRECTION('ref_axis',(1.,0.,0.));
#7026=DIRECTION('center_axis',(0.,0.,-1.));
#7027=DIRECTION('ref_axis',(1.,0.,0.));
#7028=DIRECTION('center_axis',(0.,0.,-1.));
#7029=DIRECTION('ref_axis',(1.,0.,0.));
#7030=DIRECTION('',(0.,0.,-1.));
#7031=DIRECTION('center_axis',(0.,0.,1.));
#7032=DIRECTION('ref_axis',(1.,0.,0.));
#7033=DIRECTION('center_axis',(0.,0.,-1.));
#7034=DIRECTION('ref_axis',(1.,0.,0.));
#7035=DIRECTION('center_axis',(0.,0.,-1.));
#7036=DIRECTION('ref_axis',(1.,0.,0.));
#7037=DIRECTION('',(0.,0.,-1.));
#7038=DIRECTION('center_axis',(0.,0.,1.));
#7039=DIRECTION('ref_axis',(1.,0.,0.));
#7040=DIRECTION('center_axis',(-0.499999999999999,0.866025403784439,0.));
#7041=DIRECTION('ref_axis',(-0.866025403784439,-0.499999999999999,0.));
#7042=DIRECTION('',(0.866025403784439,0.499999999999999,0.));
#7043=DIRECTION('',(0.,0.,1.));
#7044=DIRECTION('',(-0.866025403784439,-0.499999999999999,0.));
#7045=DIRECTION('',(0.,0.,1.));
#7046=DIRECTION('center_axis',(0.,0.,1.));
#7047=DIRECTION('ref_axis',(-0.866025403784439,-0.499999999999999,0.));
#7048=DIRECTION('center_axis',(0.,0.,1.));
#7049=DIRECTION('ref_axis',(-0.866025403784439,-0.499999999999999,0.));
#7050=DIRECTION('center_axis',(0.,0.,-1.));
#7051=DIRECTION('ref_axis',(-0.866025403784439,-0.499999999999999,0.));
#7052=DIRECTION('',(0.,0.,1.));
#7053=DIRECTION('center_axis',(0.994521895368273,-0.104528463267654,0.));
#7054=DIRECTION('ref_axis',(0.104528463267654,0.994521895368273,0.));
#7055=DIRECTION('',(-0.104528463267654,-0.994521895368273,0.));
#7056=DIRECTION('',(0.104528463267654,0.994521895368273,0.));
#7057=DIRECTION('',(0.,0.,1.));
#7058=DIRECTION('center_axis',(0.,0.,1.));
#7059=DIRECTION('ref_axis',(-0.866025403784439,-0.499999999999999,0.));
#7060=DIRECTION('center_axis',(0.,0.,-1.));
#7061=DIRECTION('ref_axis',(-0.866025403784439,-0.499999999999999,0.));
#7062=DIRECTION('center_axis',(0.,0.,1.));
#7063=DIRECTION('ref_axis',(-0.866025403784439,-0.499999999999999,0.));
#7064=DIRECTION('center_axis',(0.,0.,1.));
#7065=DIRECTION('ref_axis',(0.499999999999999,-0.866025403784439,0.));
#7066=DIRECTION('center_axis',(0.5,0.866025403784438,0.));
#7067=DIRECTION('ref_axis',(-0.866025403784438,0.5,0.));
#7068=DIRECTION('',(0.866025403784438,-0.5,0.));
#7069=DIRECTION('',(0.,0.,1.));
#7070=DIRECTION('',(-0.866025403784438,0.5,0.));
#7071=DIRECTION('',(0.,0.,1.));
#7072=DIRECTION('center_axis',(0.,0.,1.));
#7073=DIRECTION('ref_axis',(-0.866025403784438,0.5,0.));
#7074=DIRECTION('center_axis',(0.,0.,1.));
#7075=DIRECTION('ref_axis',(-0.866025403784438,0.5,0.));
#7076=DIRECTION('center_axis',(0.,0.,-1.));
#7077=DIRECTION('ref_axis',(-0.866025403784438,0.5,0.));
#7078=DIRECTION('',(0.,0.,1.));
#7079=DIRECTION('center_axis',(0.4067366430758,-0.913545457642601,0.));
#7080=DIRECTION('ref_axis',(0.913545457642601,0.4067366430758,0.));
#7081=DIRECTION('',(-0.913545457642601,-0.4067366430758,0.));
#7082=DIRECTION('',(0.913545457642601,0.4067366430758,0.));
#7083=DIRECTION('',(0.,0.,1.));
#7084=DIRECTION('center_axis',(0.,0.,1.));
#7085=DIRECTION('ref_axis',(-0.866025403784438,0.5,0.));
#7086=DIRECTION('center_axis',(0.,0.,-1.));
#7087=DIRECTION('ref_axis',(-0.866025403784438,0.5,0.));
#7088=DIRECTION('center_axis',(0.,0.,1.));
#7089=DIRECTION('ref_axis',(-0.866025403784438,0.5,0.));
#7090=DIRECTION('center_axis',(0.,0.,1.));
#7091=DIRECTION('ref_axis',(-0.5,-0.866025403784438,0.));
#7092=DIRECTION('center_axis',(1.,-1.66533453693773E-16,0.));
#7093=DIRECTION('ref_axis',(1.66533453693773E-16,1.,0.));
#7094=DIRECTION('',(-1.66533453693773E-16,-1.,0.));
#7095=DIRECTION('',(0.,0.,1.));
#7096=DIRECTION('',(1.66533453693773E-16,1.,0.));
#7097=DIRECTION('',(0.,0.,1.));
#7098=DIRECTION('center_axis',(0.,0.,1.));
#7099=DIRECTION('ref_axis',(1.53134210293125E-16,1.,0.));
#7100=DIRECTION('center_axis',(0.,0.,1.));
#7101=DIRECTION('ref_axis',(1.53134210293125E-16,1.,0.));
#7102=DIRECTION('center_axis',(0.,0.,-1.));
#7103=DIRECTION('ref_axis',(1.53134210293125E-16,1.,0.));
#7104=DIRECTION('',(0.,0.,1.));
#7105=DIRECTION('center_axis',(-0.587785252292473,-0.809016994374947,0.));
#7106=DIRECTION('ref_axis',(0.809016994374947,-0.587785252292473,0.));
#7107=DIRECTION('',(-0.809016994374947,0.587785252292473,0.));
#7108=DIRECTION('',(0.809016994374947,-0.587785252292473,0.));
#7109=DIRECTION('',(0.,0.,1.));
#7110=DIRECTION('center_axis',(0.,0.,1.));
#7111=DIRECTION('ref_axis',(-6.93889390390723E-17,1.,0.));
#7112=DIRECTION('center_axis',(0.,0.,-1.));
#7113=DIRECTION('ref_axis',(-6.93889390390723E-17,1.,0.));
#7114=DIRECTION('center_axis',(0.,0.,1.));
#7115=DIRECTION('ref_axis',(-6.93889390390723E-17,1.,0.));
#7116=DIRECTION('center_axis',(0.,0.,1.));
#7117=DIRECTION('ref_axis',(-1.,1.66533453693773E-16,0.));
#7118=DIRECTION('center_axis',(0.5,-0.866025403784439,0.));
#7119=DIRECTION('ref_axis',(0.866025403784439,0.5,0.));
#7120=DIRECTION('',(-0.866025403784439,-0.5,0.));
#7121=DIRECTION('',(0.,0.,1.));
#7122=DIRECTION('',(0.866025403784439,0.5,0.));
#7123=DIRECTION('',(0.,0.,1.));
#7124=DIRECTION('center_axis',(0.,0.,1.));
#7125=DIRECTION('ref_axis',(0.866025403784439,0.5,0.));
#7126=DIRECTION('center_axis',(0.,0.,1.));
#7127=DIRECTION('ref_axis',(0.866025403784439,0.5,0.));
#7128=DIRECTION('center_axis',(0.,0.,-1.));
#7129=DIRECTION('ref_axis',(0.866025403784439,0.5,0.));
#7130=DIRECTION('',(0.,0.,1.));
#7131=DIRECTION('center_axis',(-0.994521895368273,0.104528463267654,0.));
#7132=DIRECTION('ref_axis',(-0.104528463267654,-0.994521895368273,0.));
#7133=DIRECTION('',(0.104528463267654,0.994521895368273,0.));
#7134=DIRECTION('',(-0.104528463267654,-0.994521895368273,0.));
#7135=DIRECTION('',(0.,0.,1.));
#7136=DIRECTION('center_axis',(0.,0.,1.));
#7137=DIRECTION('ref_axis',(0.866025403784439,0.5,0.));
#7138=DIRECTION('center_axis',(0.,0.,-1.));
#7139=DIRECTION('ref_axis',(0.866025403784439,0.5,0.));
#7140=DIRECTION('center_axis',(0.,0.,1.));
#7141=DIRECTION('ref_axis',(0.866025403784439,0.5,0.));
#7142=DIRECTION('center_axis',(0.,0.,1.));
#7143=DIRECTION('ref_axis',(-0.5,0.866025403784439,0.));
#7144=DIRECTION('center_axis',(-0.5,-0.866025403784439,0.));
#7145=DIRECTION('ref_axis',(0.866025403784439,-0.5,0.));
#7146=DIRECTION('',(-0.866025403784439,0.5,0.));
#7147=DIRECTION('',(0.,0.,1.));
#7148=DIRECTION('',(0.866025403784439,-0.5,0.));
#7149=DIRECTION('',(0.,0.,1.));
#7150=DIRECTION('center_axis',(0.,0.,1.));
#7151=DIRECTION('ref_axis',(0.866025403784439,-0.5,0.));
#7152=DIRECTION('center_axis',(0.,0.,1.));
#7153=DIRECTION('ref_axis',(0.866025403784439,-0.5,0.));
#7154=DIRECTION('center_axis',(0.,0.,-1.));
#7155=DIRECTION('ref_axis',(0.866025403784439,-0.5,0.));
#7156=DIRECTION('',(0.,0.,1.));
#7157=DIRECTION('center_axis',(-0.4067366430758,0.913545457642601,0.));
#7158=DIRECTION('ref_axis',(-0.913545457642601,-0.4067366430758,0.));
#7159=DIRECTION('',(0.913545457642601,0.4067366430758,0.));
#7160=DIRECTION('',(-0.913545457642601,-0.4067366430758,0.));
#7161=DIRECTION('',(0.,0.,1.));
#7162=DIRECTION('center_axis',(0.,0.,1.));
#7163=DIRECTION('ref_axis',(0.866025403784439,-0.5,0.));
#7164=DIRECTION('center_axis',(0.,0.,-1.));
#7165=DIRECTION('ref_axis',(0.866025403784439,-0.5,0.));
#7166=DIRECTION('center_axis',(0.,0.,1.));
#7167=DIRECTION('ref_axis',(0.866025403784439,-0.5,0.));
#7168=DIRECTION('center_axis',(0.,0.,1.));
#7169=DIRECTION('ref_axis',(0.5,0.866025403784439,0.));
#7170=DIRECTION('center_axis',(-1.,0.,0.));
#7171=DIRECTION('ref_axis',(0.,-1.,0.));
#7172=DIRECTION('',(0.,1.,0.));
#7173=DIRECTION('',(0.,0.,1.));
#7174=DIRECTION('',(0.,-1.,0.));
#7175=DIRECTION('',(0.,0.,1.));
#7176=DIRECTION('center_axis',(0.,0.,1.));
#7177=DIRECTION('ref_axis',(0.,-1.,0.));
#7178=DIRECTION('center_axis',(0.,0.,1.));
#7179=DIRECTION('ref_axis',(0.,-1.,0.));
#7180=DIRECTION('center_axis',(0.,0.,-1.));
#7181=DIRECTION('ref_axis',(0.,-1.,0.));
#7182=DIRECTION('',(0.,0.,1.));
#7183=DIRECTION('center_axis',(0.587785252292473,0.809016994374947,0.));
#7184=DIRECTION('ref_axis',(-0.809016994374947,0.587785252292473,0.));
#7185=DIRECTION('',(0.809016994374947,-0.587785252292473,0.));
#7186=DIRECTION('',(-0.809016994374947,0.587785252292473,0.));
#7187=DIRECTION('',(0.,0.,1.));
#7188=DIRECTION('center_axis',(0.,0.,1.));
#7189=DIRECTION('ref_axis',(1.38777878078145E-16,-1.,0.));
#7190=DIRECTION('center_axis',(0.,0.,-1.));
#7191=DIRECTION('ref_axis',(1.38777878078145E-16,-1.,0.));
#7192=DIRECTION('center_axis',(0.,0.,1.));
#7193=DIRECTION('ref_axis',(1.38777878078145E-16,-1.,0.));
#7194=DIRECTION('center_axis',(0.,0.,1.));
#7195=DIRECTION('ref_axis',(1.,0.,0.));
#7196=DIRECTION('center_axis',(0.866025403784438,-0.5,0.));
#7197=DIRECTION('ref_axis',(0.5,0.866025403784438,0.));
#7198=DIRECTION('',(0.,0.,-1.));
#7199=DIRECTION('',(0.5,0.866025403784438,0.));
#7200=DIRECTION('',(0.,0.,1.));
#7201=DIRECTION('',(0.5,0.866025403784438,0.));
#7202=DIRECTION('center_axis',(-0.866025403784438,0.5,0.));
#7203=DIRECTION('ref_axis',(-0.5,-0.866025403784438,0.));
#7204=DIRECTION('',(0.,0.,1.));
#7205=DIRECTION('',(-0.5,-0.866025403784438,0.));
#7206=DIRECTION('',(0.,0.,-1.));
#7207=DIRECTION('',(-0.5,-0.866025403784438,0.));
#7208=DIRECTION('center_axis',(-0.866025403784439,-0.5,0.));
#7209=DIRECTION('ref_axis',(0.5,-0.866025403784439,0.));
#7210=DIRECTION('',(0.,0.,-1.));
#7211=DIRECTION('',(0.5,-0.866025403784439,0.));
#7212=DIRECTION('',(0.,0.,1.));
#7213=DIRECTION('',(0.5,-0.866025403784439,0.));
#7214=DIRECTION('center_axis',(0.866025403784439,0.5,0.));
#7215=DIRECTION('ref_axis',(-0.5,0.866025403784439,0.));
#7216=DIRECTION('',(0.,0.,1.));
#7217=DIRECTION('',(-0.5,0.866025403784439,0.));
#7218=DIRECTION('',(0.,0.,-1.));
#7219=DIRECTION('',(-0.5,0.866025403784439,0.));
#7220=DIRECTION('center_axis',(0.,0.,1.));
#7221=DIRECTION('ref_axis',(1.,0.,0.));
#7222=DIRECTION('center_axis',(0.,0.,1.));
#7223=DIRECTION('ref_axis',(1.,0.,0.));
#7224=DIRECTION('center_axis',(0.,0.,1.));
#7225=DIRECTION('ref_axis',(1.,0.,0.));
#7226=DIRECTION('center_axis',(0.,0.,1.));
#7227=DIRECTION('ref_axis',(1.,0.,0.));
#7228=DIRECTION('',(-1.,0.,0.));
#7229=DIRECTION('center_axis',(0.,0.,1.));
#7230=DIRECTION('ref_axis',(1.,0.,0.));
#7231=DIRECTION('',(1.,0.,0.));
#7232=DIRECTION('center_axis',(0.,0.,1.));
#7233=DIRECTION('ref_axis',(1.,0.,0.));
#7234=DIRECTION('center_axis',(0.,0.,1.));
#7235=DIRECTION('ref_axis',(1.,0.,0.));
#7236=DIRECTION('center_axis',(0.,0.,-1.));
#7237=DIRECTION('ref_axis',(1.,0.,0.));
#7238=DIRECTION('center_axis',(0.,0.,1.));
#7239=DIRECTION('ref_axis',(1.,0.,0.));
#7240=DIRECTION('center_axis',(0.,0.,1.));
#7241=DIRECTION('ref_axis',(1.,0.,0.));
#7242=DIRECTION('',(0.,0.,1.));
#7243=DIRECTION('center_axis',(0.,0.,1.));
#7244=DIRECTION('ref_axis',(-1.,7.6571373978539E-16,0.));
#7245=DIRECTION('center_axis',(0.,0.,1.));
#7246=DIRECTION('ref_axis',(1.,0.,0.));
#7247=DIRECTION('center_axis',(0.,0.,1.));
#7248=DIRECTION('ref_axis',(1.,0.,0.));
#7249=DIRECTION('',(0.,0.,-1.));
#7250=DIRECTION('center_axis',(0.,0.,1.));
#7251=DIRECTION('ref_axis',(1.,0.,0.));
#7252=DIRECTION('center_axis',(0.,0.,1.));
#7253=DIRECTION('ref_axis',(1.,0.,0.));
#7254=DIRECTION('center_axis',(0.,0.,-1.));
#7255=DIRECTION('ref_axis',(1.,0.,0.));
#7256=DIRECTION('',(0.,0.,-1.));
#7257=DIRECTION('center_axis',(0.,0.,1.));
#7258=DIRECTION('ref_axis',(1.,0.,0.));
#7259=DIRECTION('',(1.,0.,0.));
#7260=DIRECTION('center_axis',(0.,0.,-1.));
#7261=DIRECTION('ref_axis',(1.,0.,0.));
#7262=DIRECTION('',(-1.,0.,0.));
#7263=DIRECTION('center_axis',(0.,0.,-1.));
#7264=DIRECTION('ref_axis',(1.,0.,0.));
#7265=DIRECTION('center_axis',(0.,0.,-1.));
#7266=DIRECTION('ref_axis',(1.,0.,0.));
#7267=DIRECTION('center_axis',(0.,-1.,0.));
#7268=DIRECTION('ref_axis',(1.,0.,0.));
#7269=DIRECTION('',(0.,0.,-1.));
#7270=DIRECTION('center_axis',(0.,1.,0.));
#7271=DIRECTION('ref_axis',(-1.,0.,0.));
#7272=DIRECTION('',(0.,0.,1.));
#7273=DIRECTION('center_axis',(0.,0.,1.));
#7274=DIRECTION('ref_axis',(1.,0.,0.));
#7275=DIRECTION('',(0.,0.,-1.));
#7276=DIRECTION('center_axis',(0.,0.,-1.));
#7277=DIRECTION('ref_axis',(1.,0.,0.));
#7278=DIRECTION('center_axis',(0.,0.,1.));
#7279=DIRECTION('ref_axis',(1.,0.,0.));
#7280=DIRECTION('center_axis',(0.,0.,1.));
#7281=DIRECTION('ref_axis',(1.,0.,0.));
#7282=DIRECTION('',(0.,0.,-1.));
#7283=DIRECTION('center_axis',(0.,0.,1.));
#7284=DIRECTION('ref_axis',(1.,0.,0.));
#7285=DIRECTION('center_axis',(0.,0.,1.));
#7286=DIRECTION('ref_axis',(1.,0.,0.));
#7287=DIRECTION('center_axis',(0.,0.,1.));
#7288=DIRECTION('ref_axis',(1.,0.,0.));
#7289=DIRECTION('axis',(0.,0.,1.));
#7290=DIRECTION('refdir',(1.,0.,0.));
#7291=DIRECTION('center_axis',(0.,0.,-1.));
#7292=DIRECTION('ref_axis',(1.,0.,0.));
#7293=DIRECTION('center_axis',(0.,0.,1.));
#7294=DIRECTION('ref_axis',(1.,0.,0.));
#7295=DIRECTION('',(0.,0.,-1.));
#7296=DIRECTION('center_axis',(0.,0.,1.));
#7297=DIRECTION('ref_axis',(1.,0.,0.));
#7298=DIRECTION('center_axis',(0.,0.,-1.));
#7299=DIRECTION('ref_axis',(1.,0.,0.));
#7300=DIRECTION('center_axis',(0.,0.,-1.));
#7301=DIRECTION('ref_axis',(1.,0.,0.));
#7302=DIRECTION('',(0.,0.,-1.));
#7303=DIRECTION('center_axis',(0.,0.,-1.));
#7304=DIRECTION('ref_axis',(1.,0.,0.));
#7305=DIRECTION('center_axis',(0.,0.,1.));
#7306=DIRECTION('ref_axis',(1.,0.,0.));
#7307=DIRECTION('center_axis',(0.,0.,1.));
#7308=DIRECTION('ref_axis',(1.,0.,0.));
#7309=DIRECTION('center_axis',(0.,0.,-1.));
#7310=DIRECTION('ref_axis',(1.,0.,0.));
#7311=DIRECTION('center_axis',(0.,0.,-1.));
#7312=DIRECTION('ref_axis',(1.,0.,0.));
#7313=DIRECTION('center_axis',(0.,0.,-1.));
#7314=DIRECTION('ref_axis',(1.,0.,0.));
#7315=DIRECTION('',(0.,0.,-1.));
#7316=DIRECTION('center_axis',(0.,0.,1.));
#7317=DIRECTION('ref_axis',(1.,0.,0.));
#7318=DIRECTION('center_axis',(0.,0.,-1.));
#7319=DIRECTION('ref_axis',(1.,0.,0.));
#7320=DIRECTION('center_axis',(0.,0.,-1.));
#7321=DIRECTION('ref_axis',(1.,0.,0.));
#7322=DIRECTION('',(0.,0.,-1.));
#7323=DIRECTION('center_axis',(0.,0.,1.));
#7324=DIRECTION('ref_axis',(1.,0.,0.));
#7325=DIRECTION('center_axis',(0.,0.,-1.));
#7326=DIRECTION('ref_axis',(1.,0.,0.));
#7327=DIRECTION('center_axis',(0.,0.,-1.));
#7328=DIRECTION('ref_axis',(1.,0.,0.));
#7329=DIRECTION('',(0.,0.,-1.));
#7330=DIRECTION('center_axis',(0.,0.,1.));
#7331=DIRECTION('ref_axis',(1.,0.,0.));
#7332=DIRECTION('center_axis',(0.,0.,-1.));
#7333=DIRECTION('ref_axis',(1.,0.,0.));
#7334=DIRECTION('center_axis',(0.,0.,-1.));
#7335=DIRECTION('ref_axis',(1.,0.,0.));
#7336=DIRECTION('',(0.,0.,-1.));
#7337=DIRECTION('center_axis',(0.,0.,1.));
#7338=DIRECTION('ref_axis',(1.,0.,0.));
#7339=DIRECTION('center_axis',(0.,0.,1.));
#7340=DIRECTION('ref_axis',(1.,0.,0.));
#7341=DIRECTION('',(0.,0.,-1.));
#7342=DIRECTION('center_axis',(0.,0.,-1.));
#7343=DIRECTION('ref_axis',(1.,0.,0.));
#7344=DIRECTION('center_axis',(0.,0.,1.));
#7345=DIRECTION('ref_axis',(1.,0.,0.));
#7346=DIRECTION('center_axis',(0.,0.,1.));
#7347=DIRECTION('ref_axis',(1.,0.,0.));
#7348=DIRECTION('',(0.,0.,-1.));
#7349=DIRECTION('center_axis',(0.,0.,1.));
#7350=DIRECTION('ref_axis',(1.,0.,0.));
#7351=DIRECTION('center_axis',(0.,0.,1.));
#7352=DIRECTION('ref_axis',(1.,0.,0.));
#7353=DIRECTION('center_axis',(0.,0.,1.));
#7354=DIRECTION('ref_axis',(1.,0.,0.));
#7355=DIRECTION('axis',(0.,0.,1.));
#7356=DIRECTION('refdir',(1.,0.,0.));
#7357=DIRECTION('center_axis',(0.,-1.,0.));
#7358=DIRECTION('ref_axis',(-1.,0.,0.));
#7359=DIRECTION('',(0.,0.,-1.));
#7360=DIRECTION('',(1.,0.,0.));
#7361=DIRECTION('',(0.,0.,-1.));
#7362=DIRECTION('',(1.,0.,0.));
#7363=DIRECTION('center_axis',(1.,0.,0.));
#7364=DIRECTION('ref_axis',(0.,-1.,0.));
#7365=DIRECTION('',(0.,1.,0.));
#7366=DIRECTION('',(0.,0.,-1.));
#7367=DIRECTION('',(0.,1.,0.));
#7368=DIRECTION('center_axis',(0.,1.,0.));
#7369=DIRECTION('ref_axis',(1.,0.,0.));
#7370=DIRECTION('',(0.,0.,1.));
#7371=DIRECTION('',(-1.,0.,0.));
#7372=DIRECTION('',(-1.,0.,0.));
#7373=DIRECTION('center_axis',(0.,0.,1.));
#7374=DIRECTION('ref_axis',(1.,0.,0.));
#7375=DIRECTION('center_axis',(0.,0.,-1.));
#7376=DIRECTION('ref_axis',(1.,0.,0.));
#7377=DIRECTION('center_axis',(0.,0.,1.));
#7378=DIRECTION('ref_axis',(1.,0.,0.));
#7379=DIRECTION('center_axis',(0.,0.,1.));
#7380=DIRECTION('ref_axis',(1.,0.,0.));
#7381=DIRECTION('center_axis',(0.,0.,-1.));
#7382=DIRECTION('ref_axis',(0.913545457642601,-0.406736643075801,0.));
#7383=DIRECTION('',(0.913545457642601,-0.406736643075801,0.));
#7384=DIRECTION('center_axis',(0.,0.,1.));
#7385=DIRECTION('ref_axis',(0.9135454576426,-0.406736643075801,0.));
#7386=DIRECTION('',(-0.866025403784439,-0.499999999999999,0.));
#7387=DIRECTION('center_axis',(0.,0.,-1.));
#7388=DIRECTION('ref_axis',(0.104528463267653,-0.994521895368273,0.));
#7389=DIRECTION('',(0.104528463267653,-0.994521895368273,0.));
#7390=DIRECTION('center_axis',(0.,0.,1.));
#7391=DIRECTION('ref_axis',(0.104528463267653,-0.994521895368274,0.));
#7392=DIRECTION('',(-0.866025403784438,0.5,0.));
#7393=DIRECTION('center_axis',(0.,0.,-1.));
#7394=DIRECTION('ref_axis',(-0.809016994374948,-0.587785252292473,0.));
#7395=DIRECTION('',(-0.809016994374947,-0.587785252292473,0.));
#7396=DIRECTION('center_axis',(0.,0.,1.));
#7397=DIRECTION('ref_axis',(-0.809016994374948,-0.587785252292473,0.));
#7398=DIRECTION('',(1.66533453693773E-16,1.,0.));
#7399=DIRECTION('center_axis',(0.,0.,-1.));
#7400=DIRECTION('ref_axis',(-0.913545457642601,0.406736643075801,0.));
#7401=DIRECTION('',(-0.913545457642601,0.4067366430758,0.));
#7402=DIRECTION('center_axis',(0.,0.,1.));
#7403=DIRECTION('ref_axis',(-0.913545457642601,0.406736643075801,0.));
#7404=DIRECTION('',(0.866025403784439,0.5,0.));
#7405=DIRECTION('center_axis',(0.,0.,-1.));
#7406=DIRECTION('ref_axis',(-0.104528463267653,0.994521895368273,0.));
#7407=DIRECTION('',(-0.104528463267653,0.994521895368273,0.));
#7408=DIRECTION('center_axis',(0.,0.,1.));
#7409=DIRECTION('ref_axis',(-0.104528463267653,0.994521895368273,0.));
#7410=DIRECTION('',(0.866025403784439,-0.5,0.));
#7411=DIRECTION('center_axis',(0.,0.,-1.));
#7412=DIRECTION('ref_axis',(0.809016994374948,0.587785252292473,0.));
#7413=DIRECTION('',(0.809016994374947,0.587785252292473,0.));
#7414=DIRECTION('center_axis',(0.,0.,1.));
#7415=DIRECTION('ref_axis',(0.809016994374948,0.587785252292473,0.));
#7416=DIRECTION('',(0.,-1.,0.));
#7417=DIRECTION('center_axis',(0.,0.,-1.));
#7418=DIRECTION('ref_axis',(1.,0.,0.));
#7419=DIRECTION('center_axis',(0.,0.,-1.));
#7420=DIRECTION('ref_axis',(1.,0.,0.));
#7421=DIRECTION('center_axis',(0.,0.,1.));
#7422=DIRECTION('ref_axis',(0.913545457642601,-0.406736643075801,0.));
#7423=DIRECTION('center_axis',(0.,0.,1.));
#7424=DIRECTION('ref_axis',(0.913545457642601,-0.406736643075801,0.));
#7425=DIRECTION('',(0.,0.,1.));
#7426=DIRECTION('',(0.,0.,1.));
#7427=DIRECTION('center_axis',(-0.499999999999999,0.866025403784439,0.));
#7428=DIRECTION('ref_axis',(-0.866025403784439,-0.499999999999999,0.));
#7429=DIRECTION('',(-0.866025403784439,-0.499999999999999,0.));
#7430=DIRECTION('',(0.,0.,1.));
#7431=DIRECTION('center_axis',(0.,0.,1.));
#7432=DIRECTION('ref_axis',(0.9135454576426,-0.406736643075801,0.));
#7433=DIRECTION('center_axis',(0.,0.,1.));
#7434=DIRECTION('ref_axis',(0.9135454576426,-0.406736643075801,0.));
#7435=DIRECTION('',(0.,0.,1.));
#7436=DIRECTION('center_axis',(-0.406736643075801,-0.913545457642601,0.));
#7437=DIRECTION('ref_axis',(0.913545457642601,-0.406736643075801,0.));
#7438=DIRECTION('',(0.913545457642601,-0.406736643075801,0.));
#7439=DIRECTION('center_axis',(0.,0.,1.));
#7440=DIRECTION('ref_axis',(0.499999999999999,-0.866025403784439,0.));
#7441=DIRECTION('center_axis',(0.,0.,1.));
#7442=DIRECTION('ref_axis',(0.104528463267653,-0.994521895368273,0.));
#7443=DIRECTION('center_axis',(0.,0.,1.));
#7444=DIRECTION('ref_axis',(0.104528463267653,-0.994521895368273,0.));
#7445=DIRECTION('',(0.,0.,1.));
#7446=DIRECTION('',(0.,0.,1.));
#7447=DIRECTION('center_axis',(0.5,0.866025403784438,0.));
#7448=DIRECTION('ref_axis',(-0.866025403784438,0.5,0.));
#7449=DIRECTION('',(-0.866025403784438,0.5,0.));
#7450=DIRECTION('',(0.,0.,1.));
#7451=DIRECTION('center_axis',(0.,0.,1.));
#7452=DIRECTION('ref_axis',(0.104528463267653,-0.994521895368274,0.));
#7453=DIRECTION('center_axis',(0.,0.,1.));
#7454=DIRECTION('ref_axis',(0.104528463267653,-0.994521895368274,0.));
#7455=DIRECTION('',(0.,0.,1.));
#7456=DIRECTION('center_axis',(-0.994521895368273,-0.104528463267653,0.));
#7457=DIRECTION('ref_axis',(0.104528463267653,-0.994521895368273,0.));
#7458=DIRECTION('',(0.104528463267653,-0.994521895368273,0.));
#7459=DIRECTION('center_axis',(0.,0.,1.));
#7460=DIRECTION('ref_axis',(-0.5,-0.866025403784438,0.));
#7461=DIRECTION('center_axis',(0.,0.,1.));
#7462=DIRECTION('ref_axis',(-0.809016994374948,-0.587785252292473,0.));
#7463=DIRECTION('center_axis',(0.,0.,1.));
#7464=DIRECTION('ref_axis',(-0.809016994374948,-0.587785252292473,0.));
#7465=DIRECTION('',(0.,0.,1.));
#7466=DIRECTION('',(0.,0.,1.));
#7467=DIRECTION('center_axis',(1.,-1.66533453693773E-16,0.));
#7468=DIRECTION('ref_axis',(1.66533453693773E-16,1.,0.));
#7469=DIRECTION('',(1.66533453693773E-16,1.,0.));
#7470=DIRECTION('',(0.,0.,1.));
#7471=DIRECTION('center_axis',(0.,0.,1.));
#7472=DIRECTION('ref_axis',(-0.809016994374948,-0.587785252292473,0.));
#7473=DIRECTION('center_axis',(0.,0.,1.));
#7474=DIRECTION('ref_axis',(-0.809016994374948,-0.587785252292473,0.));
#7475=DIRECTION('',(0.,0.,1.));
#7476=DIRECTION('center_axis',(-0.587785252292473,0.809016994374947,0.));
#7477=DIRECTION('ref_axis',(-0.809016994374947,-0.587785252292473,0.));
#7478=DIRECTION('',(-0.809016994374947,-0.587785252292473,0.));
#7479=DIRECTION('center_axis',(0.,0.,1.));
#7480=DIRECTION('ref_axis',(-1.,1.66533453693773E-16,0.));
#7481=DIRECTION('center_axis',(0.,0.,1.));
#7482=DIRECTION('ref_axis',(-0.913545457642601,0.406736643075801,0.));
#7483=DIRECTION('center_axis',(0.,0.,1.));
#7484=DIRECTION('ref_axis',(-0.913545457642601,0.406736643075801,0.));
#7485=DIRECTION('',(0.,0.,1.));
#7486=DIRECTION('',(0.,0.,1.));
#7487=DIRECTION('center_axis',(0.5,-0.866025403784439,0.));
#7488=DIRECTION('ref_axis',(0.866025403784439,0.5,0.));
#7489=DIRECTION('',(0.866025403784439,0.5,0.));
#7490=DIRECTION('',(0.,0.,1.));
#7491=DIRECTION('center_axis',(0.,0.,1.));
#7492=DIRECTION('ref_axis',(-0.913545457642601,0.406736643075801,0.));
#7493=DIRECTION('center_axis',(0.,0.,1.));
#7494=DIRECTION('ref_axis',(-0.913545457642601,0.406736643075801,0.));
#7495=DIRECTION('',(0.,0.,1.));
#7496=DIRECTION('center_axis',(0.4067366430758,0.913545457642601,0.));
#7497=DIRECTION('ref_axis',(-0.913545457642601,0.4067366430758,0.));
#7498=DIRECTION('',(-0.913545457642601,0.4067366430758,0.));
#7499=DIRECTION('center_axis',(0.,0.,1.));
#7500=DIRECTION('ref_axis',(-0.5,0.866025403784439,0.));
#7501=DIRECTION('center_axis',(0.,0.,1.));
#7502=DIRECTION('ref_axis',(-0.104528463267653,0.994521895368273,0.));
#7503=DIRECTION('center_axis',(0.,0.,1.));
#7504=DIRECTION('ref_axis',(-0.104528463267653,0.994521895368273,0.));
#7505=DIRECTION('',(0.,0.,1.));
#7506=DIRECTION('',(0.,0.,1.));
#7507=DIRECTION('center_axis',(-0.5,-0.866025403784439,0.));
#7508=DIRECTION('ref_axis',(0.866025403784439,-0.5,0.));
#7509=DIRECTION('',(0.866025403784439,-0.5,0.));
#7510=DIRECTION('',(0.,0.,1.));
#7511=DIRECTION('center_axis',(0.,0.,1.));
#7512=DIRECTION('ref_axis',(-0.104528463267653,0.994521895368273,0.));
#7513=DIRECTION('center_axis',(0.,0.,1.));
#7514=DIRECTION('ref_axis',(-0.104528463267653,0.994521895368273,0.));
#7515=DIRECTION('',(0.,0.,1.));
#7516=DIRECTION('center_axis',(0.994521895368273,0.104528463267653,0.));
#7517=DIRECTION('ref_axis',(-0.104528463267653,0.994521895368273,0.));
#7518=DIRECTION('',(-0.104528463267653,0.994521895368273,0.));
#7519=DIRECTION('center_axis',(0.,0.,1.));
#7520=DIRECTION('ref_axis',(0.5,0.866025403784439,0.));
#7521=DIRECTION('center_axis',(0.,0.,1.));
#7522=DIRECTION('ref_axis',(0.809016994374948,0.587785252292473,0.));
#7523=DIRECTION('center_axis',(0.,0.,1.));
#7524=DIRECTION('ref_axis',(0.809016994374948,0.587785252292473,0.));
#7525=DIRECTION('',(0.,0.,1.));
#7526=DIRECTION('',(0.,0.,1.));
#7527=DIRECTION('center_axis',(-1.,0.,0.));
#7528=DIRECTION('ref_axis',(0.,-1.,0.));
#7529=DIRECTION('',(0.,-1.,0.));
#7530=DIRECTION('',(0.,0.,1.));
#7531=DIRECTION('center_axis',(0.,0.,1.));
#7532=DIRECTION('ref_axis',(0.809016994374948,0.587785252292473,0.));
#7533=DIRECTION('center_axis',(0.,0.,1.));
#7534=DIRECTION('ref_axis',(0.809016994374948,0.587785252292473,0.));
#7535=DIRECTION('',(0.,0.,1.));
#7536=DIRECTION('center_axis',(0.587785252292473,-0.809016994374947,0.));
#7537=DIRECTION('ref_axis',(0.809016994374947,0.587785252292473,0.));
#7538=DIRECTION('',(0.809016994374947,0.587785252292473,0.));
#7539=DIRECTION('center_axis',(0.,0.,1.));
#7540=DIRECTION('ref_axis',(1.,0.,0.));
#7541=DIRECTION('center_axis',(0.,0.,1.));
#7542=DIRECTION('ref_axis',(1.,0.,0.));
#7543=DIRECTION('center_axis',(0.,0.,1.));
#7544=DIRECTION('ref_axis',(1.,0.,0.));
#7545=DIRECTION('',(0.,0.,-1.));
#7546=DIRECTION('center_axis',(0.,0.,-1.));
#7547=DIRECTION('ref_axis',(1.,0.,0.));
#7548=DIRECTION('center_axis',(0.,0.,1.));
#7549=DIRECTION('ref_axis',(1.,0.,0.));
#7550=DIRECTION('center_axis',(0.,0.,-1.));
#7551=DIRECTION('ref_axis',(1.,0.,0.));
#7552=DIRECTION('center_axis',(0.,0.,1.));
#7553=DIRECTION('ref_axis',(1.,0.,0.));
#7554=DIRECTION('',(0.,0.,-1.));
#7555=DIRECTION('center_axis',(0.,0.,1.));
#7556=DIRECTION('ref_axis',(1.,0.,0.));
#7557=DIRECTION('center_axis',(0.,0.,1.));
#7558=DIRECTION('ref_axis',(1.,0.,0.));
#7559=DIRECTION('',(0.,0.,-1.));
#7560=DIRECTION('center_axis',(0.,0.,1.));
#7561=DIRECTION('ref_axis',(1.,0.,0.));
#7562=DIRECTION('axis',(0.,0.,1.));
#7563=DIRECTION('refdir',(1.,0.,0.));
#7564=DIRECTION('center_axis',(0.,0.,1.));
#7565=DIRECTION('ref_axis',(1.,0.,0.));
#7566=DIRECTION('center_axis',(0.,0.,-1.));
#7567=DIRECTION('ref_axis',(1.,0.,0.));
#7568=DIRECTION('',(0.,0.,-1.));
#7569=DIRECTION('center_axis',(0.,0.,-1.));
#7570=DIRECTION('ref_axis',(1.,0.,0.));
#7571=DIRECTION('center_axis',(0.,0.,1.));
#7572=DIRECTION('ref_axis',(1.,0.,0.));
#7573=DIRECTION('center_axis',(0.,0.,1.));
#7574=DIRECTION('ref_axis',(1.,0.,0.));
#7575=DIRECTION('',(0.,0.,-1.));
#7576=DIRECTION('center_axis',(0.,0.,1.));
#7577=DIRECTION('ref_axis',(1.,0.,0.));
#7578=DIRECTION('center_axis',(0.,0.,1.));
#7579=DIRECTION('ref_axis',(1.,0.,0.));
#7580=DIRECTION('center_axis',(0.,0.,1.));
#7581=DIRECTION('ref_axis',(1.,0.,0.));
#7582=DIRECTION('axis',(0.,0.,1.));
#7583=DIRECTION('refdir',(1.,0.,0.));
#7584=DIRECTION('center_axis',(0.,0.,-1.));
#7585=DIRECTION('ref_axis',(-0.346876982621325,0.937910634830166,0.));
#7586=DIRECTION('',(0.,0.,-1.));
#7587=DIRECTION('center_axis',(0.,0.,-1.));
#7588=DIRECTION('ref_axis',(1.,0.,0.));
#7589=DIRECTION('center_axis',(0.,0.,-1.));
#7590=DIRECTION('ref_axis',(1.,0.,0.));
#7591=DIRECTION('',(0.,0.,-1.));
#7592=DIRECTION('center_axis',(0.,0.,-1.));
#7593=DIRECTION('ref_axis',(1.,0.,0.));
#7594=DIRECTION('',(0.,0.,-1.));
#7595=DIRECTION('center_axis',(0.,0.,-1.));
#7596=DIRECTION('ref_axis',(1.,0.,0.));
#7597=DIRECTION('',(0.,0.,-1.));
#7598=DIRECTION('center_axis',(0.,0.,-1.));
#7599=DIRECTION('ref_axis',(1.,0.,0.));
#7600=DIRECTION('',(0.,0.,-1.));
#7601=DIRECTION('center_axis',(0.,0.,-1.));
#7602=DIRECTION('ref_axis',(1.,0.,0.));
#7603=DIRECTION('',(0.,0.,-1.));
#7604=DIRECTION('center_axis',(0.,0.,-1.));
#7605=DIRECTION('ref_axis',(1.,0.,0.));
#7606=DIRECTION('',(0.,0.,-1.));
#7607=DIRECTION('center_axis',(0.,0.,-1.));
#7608=DIRECTION('ref_axis',(0.93800197321156,-0.346629915401454,0.));
#7609=DIRECTION('',(0.,0.,-1.));
#7610=DIRECTION('center_axis',(0.,0.,-1.));
#7611=DIRECTION('ref_axis',(1.,0.,0.));
#7612=DIRECTION('center_axis',(0.,0.,-1.));
#7613=DIRECTION('ref_axis',(-0.346877122944053,0.937910582933179,0.));
#7614=DIRECTION('',(0.,0.,-1.));
#7615=DIRECTION('center_axis',(0.,0.,-1.));
#7616=DIRECTION('ref_axis',(1.,0.,0.));
#7617=DIRECTION('center_axis',(0.,0.,-1.));
#7618=DIRECTION('ref_axis',(1.,0.,0.));
#7619=DIRECTION('',(0.,0.,-1.));
#7620=DIRECTION('center_axis',(0.,0.,-1.));
#7621=DIRECTION('ref_axis',(1.,0.,0.));
#7622=DIRECTION('',(0.,0.,-1.));
#7623=DIRECTION('center_axis',(0.,0.,-1.));
#7624=DIRECTION('ref_axis',(1.,0.,0.));
#7625=DIRECTION('',(0.,0.,-1.));
#7626=DIRECTION('center_axis',(0.,0.,-1.));
#7627=DIRECTION('ref_axis',(1.,0.,0.));
#7628=DIRECTION('',(0.,0.,-1.));
#7629=DIRECTION('center_axis',(0.,0.,-1.));
#7630=DIRECTION('ref_axis',(1.,0.,0.));
#7631=DIRECTION('',(0.,0.,-1.));
#7632=DIRECTION('center_axis',(0.,0.,-1.));
#7633=DIRECTION('ref_axis',(1.,0.,0.));
#7634=DIRECTION('',(0.,0.,-1.));
#7635=DIRECTION('center_axis',(0.,0.,-1.));
#7636=DIRECTION('ref_axis',(0.93800198232385,-0.346629890743035,0.));
#7637=DIRECTION('',(0.,0.,-1.));
#7638=DIRECTION('center_axis',(0.,0.,-1.));
#7639=DIRECTION('ref_axis',(1.,0.,0.));
#7640=DIRECTION('center_axis',(0.,0.,-1.));
#7641=DIRECTION('ref_axis',(-0.346876854373397,0.937910682261385,0.));
#7642=DIRECTION('',(0.,0.,-1.));
#7643=DIRECTION('center_axis',(0.,0.,-1.));
#7644=DIRECTION('ref_axis',(1.,0.,0.));
#7645=DIRECTION('center_axis',(0.,0.,-1.));
#7646=DIRECTION('ref_axis',(1.,0.,0.));
#7647=DIRECTION('',(0.,0.,-1.));
#7648=DIRECTION('center_axis',(0.,0.,-1.));
#7649=DIRECTION('ref_axis',(1.,0.,0.));
#7650=DIRECTION('',(0.,0.,-1.));
#7651=DIRECTION('center_axis',(0.,0.,-1.));
#7652=DIRECTION('ref_axis',(1.,0.,0.));
#7653=DIRECTION('',(0.,0.,-1.));
#7654=DIRECTION('center_axis',(0.,0.,-1.));
#7655=DIRECTION('ref_axis',(1.,0.,0.));
#7656=DIRECTION('',(0.,0.,-1.));
#7657=DIRECTION('center_axis',(0.,0.,-1.));
#7658=DIRECTION('ref_axis',(1.,0.,0.));
#7659=DIRECTION('',(0.,0.,-1.));
#7660=DIRECTION('center_axis',(0.,0.,-1.));
#7661=DIRECTION('ref_axis',(1.,0.,0.));
#7662=DIRECTION('',(0.,0.,-1.));
#7663=DIRECTION('center_axis',(0.,0.,-1.));
#7664=DIRECTION('ref_axis',(0.938001962568159,-0.346629944203154,0.));
#7665=DIRECTION('',(0.,0.,-1.));
#7666=DIRECTION('center_axis',(0.,0.,-1.));
#7667=DIRECTION('ref_axis',(1.,0.,0.));
#7668=DIRECTION('center_axis',(0.,0.,-1.));
#7669=DIRECTION('ref_axis',(-0.346877157281527,0.937910570233797,0.));
#7670=DIRECTION('',(0.,0.,-1.));
#7671=DIRECTION('center_axis',(0.,0.,-1.));
#7672=DIRECTION('ref_axis',(1.,0.,0.));
#7673=DIRECTION('center_axis',(0.,0.,-1.));
#7674=DIRECTION('ref_axis',(1.,0.,0.));
#7675=DIRECTION('',(0.,0.,-1.));
#7676=DIRECTION('center_axis',(0.,0.,-1.));
#7677=DIRECTION('ref_axis',(1.,0.,0.));
#7678=DIRECTION('',(0.,0.,-1.));
#7679=DIRECTION('center_axis',(0.,0.,-1.));
#7680=DIRECTION('ref_axis',(1.,0.,0.));
#7681=DIRECTION('',(0.,0.,-1.));
#7682=DIRECTION('center_axis',(0.,0.,-1.));
#7683=DIRECTION('ref_axis',(1.,0.,0.));
#7684=DIRECTION('',(0.,0.,-1.));
#7685=DIRECTION('center_axis',(0.,0.,-1.));
#7686=DIRECTION('ref_axis',(1.,0.,0.));
#7687=DIRECTION('',(0.,0.,-1.));
#7688=DIRECTION('center_axis',(0.,0.,-1.));
#7689=DIRECTION('ref_axis',(1.,0.,0.));
#7690=DIRECTION('',(0.,0.,-1.));
#7691=DIRECTION('center_axis',(0.,0.,-1.));
#7692=DIRECTION('ref_axis',(0.938001982323848,-0.346629890743041,0.));
#7693=DIRECTION('',(0.,0.,-1.));
#7694=DIRECTION('center_axis',(0.,0.,-1.));
#7695=DIRECTION('ref_axis',(1.,0.,0.));
#7696=DIRECTION('center_axis',(0.,0.,-1.));
#7697=DIRECTION('ref_axis',(0.793238951796279,0.608910474005121,0.));
#7698=DIRECTION('',(1.22464679914735E-16,-2.8461799209306E-30,-1.));
#7699=DIRECTION('center_axis',(0.,0.,1.));
#7700=DIRECTION('ref_axis',(1.,-2.31183580855735E-14,0.));
#7701=DIRECTION('center_axis',(0.,0.,-1.));
#7702=DIRECTION('ref_axis',(1.,-2.31183580855735E-14,0.));
#7703=DIRECTION('',(1.22464679914735E-16,-2.8461799209306E-30,-1.));
#7704=DIRECTION('center_axis',(0.,0.,-1.));
#7705=DIRECTION('ref_axis',(1.,-2.31183580855735E-14,0.));
#7706=DIRECTION('',(1.22464679914735E-16,-2.8461799209306E-30,-1.));
#7707=DIRECTION('center_axis',(0.,0.,-1.));
#7708=DIRECTION('ref_axis',(1.,-2.31183580855735E-14,0.));
#7709=DIRECTION('',(1.22464679914735E-16,-2.8461799209306E-30,-1.));
#7710=DIRECTION('center_axis',(0.,0.,-1.));
#7711=DIRECTION('ref_axis',(1.,-2.31183580855735E-14,0.));
#7712=DIRECTION('',(1.22464679914735E-16,-2.8461799209306E-30,-1.));
#7713=DIRECTION('center_axis',(0.,0.,-1.));
#7714=DIRECTION('ref_axis',(1.,-2.31183580855735E-14,0.));
#7715=DIRECTION('',(1.22464679914735E-16,-2.8461799209306E-30,-1.));
#7716=DIRECTION('center_axis',(0.,0.,-1.));
#7717=DIRECTION('ref_axis',(1.,-2.31183580855735E-14,0.));
#7718=DIRECTION('',(1.22464679914735E-16,-2.8461799209306E-30,-1.));
#7719=DIRECTION('center_axis',(0.,0.,-1.));
#7720=DIRECTION('ref_axis',(-0.609093803263995,-0.793098189901731,0.));
#7721=DIRECTION('',(1.22464679914735E-16,-2.8461799209306E-30,-1.));
#7722=DIRECTION('center_axis',(0.,0.,-1.));
#7723=DIRECTION('ref_axis',(1.,-2.31183580855735E-14,0.));
#7724=DIRECTION('center_axis',(0.,0.,-1.));
#7725=DIRECTION('ref_axis',(0.793238910128574,0.608910528286408,0.));
#7726=DIRECTION('',(1.22464679914735E-16,-2.2355846543427E-30,-1.));
#7727=DIRECTION('center_axis',(0.,0.,1.));
#7728=DIRECTION('ref_axis',(1.,-1.81324693622859E-14,0.));
#7729=DIRECTION('center_axis',(0.,0.,-1.));
#7730=DIRECTION('ref_axis',(1.,-1.81324693622859E-14,0.));
#7731=DIRECTION('',(1.22464679914735E-16,-2.2355846543427E-30,-1.));
#7732=DIRECTION('center_axis',(0.,0.,-1.));
#7733=DIRECTION('ref_axis',(1.,-1.81324693622859E-14,0.));
#7734=DIRECTION('',(1.22464679914735E-16,-2.2355846543427E-30,-1.));
#7735=DIRECTION('center_axis',(0.,0.,-1.));
#7736=DIRECTION('ref_axis',(1.,-1.81324693622859E-14,0.));
#7737=DIRECTION('',(1.22464679914735E-16,-2.2355846543427E-30,-1.));
#7738=DIRECTION('center_axis',(0.,0.,-1.));
#7739=DIRECTION('ref_axis',(1.,-1.81324693622859E-14,0.));
#7740=DIRECTION('',(1.22464679914735E-16,-2.2355846543427E-30,-1.));
#7741=DIRECTION('center_axis',(0.,0.,-1.));
#7742=DIRECTION('ref_axis',(1.,-1.81324693622859E-14,0.));
#7743=DIRECTION('',(1.22464679914735E-16,-2.2355846543427E-30,-1.));
#7744=DIRECTION('center_axis',(0.,0.,-1.));
#7745=DIRECTION('ref_axis',(1.,-1.81324693622859E-14,0.));
#7746=DIRECTION('',(1.22464679914735E-16,-2.2355846543427E-30,-1.));
#7747=DIRECTION('center_axis',(0.,0.,-1.));
#7748=DIRECTION('ref_axis',(-0.609093787363252,-0.793098202113388,0.));
#7749=DIRECTION('',(1.22464679914735E-16,-2.2355846543427E-30,-1.));
#7750=DIRECTION('center_axis',(0.,0.,-1.));
#7751=DIRECTION('ref_axis',(1.,-1.81324693622859E-14,0.));
#7752=DIRECTION('center_axis',(0.,0.,-1.));
#7753=DIRECTION('ref_axis',(0.793238959206298,0.608910464351951,0.));
#7754=DIRECTION('',(1.22464679914735E-16,-2.23556116661122E-30,-1.));
#7755=DIRECTION('center_axis',(0.,0.,1.));
#7756=DIRECTION('ref_axis',(1.,-1.81322775704035E-14,0.));
#7757=DIRECTION('center_axis',(0.,0.,-1.));
#7758=DIRECTION('ref_axis',(1.,-1.81322775704035E-14,0.));
#7759=DIRECTION('',(1.22464679914735E-16,-2.23556116661122E-30,-1.));
#7760=DIRECTION('center_axis',(0.,0.,-1.));
#7761=DIRECTION('ref_axis',(1.,-1.81322775704035E-14,0.));
#7762=DIRECTION('',(1.22464679914735E-16,-2.23556116661122E-30,-1.));
#7763=DIRECTION('center_axis',(0.,0.,-1.));
#7764=DIRECTION('ref_axis',(1.,-1.81322775704035E-14,0.));
#7765=DIRECTION('',(1.22464679914735E-16,-2.23556116661122E-30,-1.));
#7766=DIRECTION('center_axis',(0.,0.,-1.));
#7767=DIRECTION('ref_axis',(1.,-1.81322775704035E-14,0.));
#7768=DIRECTION('',(1.22464679914735E-16,-2.23556116661122E-30,-1.));
#7769=DIRECTION('center_axis',(0.,0.,-1.));
#7770=DIRECTION('ref_axis',(1.,-1.81322775704035E-14,0.));
#7771=DIRECTION('',(1.22464679914735E-16,-2.23556116661122E-30,-1.));
#7772=DIRECTION('center_axis',(0.,0.,-1.));
#7773=DIRECTION('ref_axis',(1.,-1.81322775704035E-14,0.));
#7774=DIRECTION('',(1.22464679914735E-16,-2.23556116661122E-30,-1.));
#7775=DIRECTION('center_axis',(0.,0.,-1.));
#7776=DIRECTION('ref_axis',(-0.609093821447985,-0.793098175936555,0.));
#7777=DIRECTION('',(1.22464679914735E-16,-2.23556116661122E-30,-1.));
#7778=DIRECTION('center_axis',(0.,0.,-1.));
#7779=DIRECTION('ref_axis',(1.,-1.81322775704035E-14,0.));
#7780=DIRECTION('center_axis',(0.,0.,-1.));
#7781=DIRECTION('ref_axis',(0.793238929068431,0.608910503613107,0.));
#7782=DIRECTION('',(1.22464679914735E-16,-1.43058875937861E-30,-1.));
#7783=DIRECTION('center_axis',(0.,0.,1.));
#7784=DIRECTION('ref_axis',(1.,-1.15591790427867E-14,0.));
#7785=DIRECTION('center_axis',(0.,0.,-1.));
#7786=DIRECTION('ref_axis',(1.,-1.15591790427867E-14,0.));
#7787=DIRECTION('',(1.22464679914735E-16,-1.43058875937861E-30,-1.));
#7788=DIRECTION('center_axis',(0.,0.,-1.));
#7789=DIRECTION('ref_axis',(1.,-1.15591790427867E-14,0.));
#7790=DIRECTION('',(1.22464679914735E-16,-1.43058875937861E-30,-1.));
#7791=DIRECTION('center_axis',(0.,0.,-1.));
#7792=DIRECTION('ref_axis',(1.,-1.15591790427867E-14,0.));
#7793=DIRECTION('',(1.22464679914735E-16,-1.43058875937861E-30,-1.));
#7794=DIRECTION('center_axis',(0.,0.,-1.));
#7795=DIRECTION('ref_axis',(1.,-1.15591790427867E-14,0.));
#7796=DIRECTION('',(1.22464679914735E-16,-1.43058875937861E-30,-1.));
#7797=DIRECTION('center_axis',(0.,0.,-1.));
#7798=DIRECTION('ref_axis',(1.,-1.15591790427867E-14,0.));
#7799=DIRECTION('',(1.22464679914735E-16,-1.43058875937861E-30,-1.));
#7800=DIRECTION('center_axis',(0.,0.,-1.));
#7801=DIRECTION('ref_axis',(1.,-1.15591790427867E-14,0.));
#7802=DIRECTION('',(1.22464679914735E-16,-1.43058875937861E-30,-1.));
#7803=DIRECTION('center_axis',(0.,0.,-1.));
#7804=DIRECTION('ref_axis',(-0.609093787363245,-0.793098202113394,0.));
#7805=DIRECTION('',(1.22464679914735E-16,-1.43058875937861E-30,-1.));
#7806=DIRECTION('center_axis',(0.,0.,-1.));
#7807=DIRECTION('ref_axis',(1.,-1.15591790427867E-14,0.));
#7808=DIRECTION('center_axis',(0.,0.,-1.));
#7809=DIRECTION('ref_axis',(1.,0.,0.));
#7810=DIRECTION('center_axis',(0.,0.,1.));
#7811=DIRECTION('ref_axis',(1.,0.,0.));
#7812=DIRECTION('',(0.,0.,-1.));
#7813=DIRECTION('center_axis',(0.,0.,1.));
#7814=DIRECTION('ref_axis',(1.,0.,0.));
#7815=DIRECTION('center_axis',(0.,0.,-1.));
#7816=DIRECTION('ref_axis',(1.,0.,0.));
#7817=DIRECTION('center_axis',(0.,0.,-1.));
#7818=DIRECTION('ref_axis',(1.,0.,0.));
#7819=DIRECTION('',(0.,0.,-1.));
#7820=DIRECTION('center_axis',(0.,0.,-1.));
#7821=DIRECTION('ref_axis',(1.,0.,0.));
#7822=DIRECTION('center_axis',(0.,0.,1.));
#7823=DIRECTION('ref_axis',(1.,0.,0.));
#7824=DIRECTION('center_axis',(0.,0.,1.));
#7825=DIRECTION('ref_axis',(1.,0.,0.));
#7826=DIRECTION('center_axis',(0.,0.,-1.));
#7827=DIRECTION('ref_axis',(1.,0.,0.));
#7828=DIRECTION('center_axis',(0.,0.,-1.));
#7829=DIRECTION('ref_axis',(1.,0.,0.));
#7830=DIRECTION('',(0.5,-0.866025403784439,0.));
#7831=DIRECTION('center_axis',(0.,0.,1.));
#7832=DIRECTION('ref_axis',(1.,0.,0.));
#7833=DIRECTION('',(-0.5,-0.866025403784438,0.));
#7834=DIRECTION('center_axis',(0.,0.,-1.));
#7835=DIRECTION('ref_axis',(1.,0.,0.));
#7836=DIRECTION('',(-1.,0.,0.));
#7837=DIRECTION('center_axis',(0.,0.,1.));
#7838=DIRECTION('ref_axis',(1.,0.,0.));
#7839=DIRECTION('',(-0.5,0.866025403784439,0.));
#7840=DIRECTION('',(0.5,0.866025403784438,0.));
#7841=DIRECTION('center_axis',(0.,0.,1.));
#7842=DIRECTION('ref_axis',(1.,0.,0.));
#7843=DIRECTION('',(1.,0.,0.));
#7844=DIRECTION('center_axis',(0.,0.,-1.));
#7845=DIRECTION('ref_axis',(1.,0.,0.));
#7846=DIRECTION('center_axis',(0.,0.,-1.));
#7847=DIRECTION('ref_axis',(1.,0.,0.));
#7848=DIRECTION('center_axis',(0.,0.,-1.));
#7849=DIRECTION('ref_axis',(1.,-1.15591790427867E-14,0.));
#7850=DIRECTION('center_axis',(0.,0.,1.));
#7851=DIRECTION('ref_axis',(1.,0.,0.));
#7852=DIRECTION('center_axis',(0.,0.,1.));
#7853=DIRECTION('ref_axis',(1.,0.,0.));
#7854=DIRECTION('center_axis',(0.,0.,1.));
#7855=DIRECTION('ref_axis',(1.,0.,0.));
#7856=DIRECTION('center_axis',(0.,0.,-1.));
#7857=DIRECTION('ref_axis',(1.,-1.81322775704035E-14,0.));
#7858=DIRECTION('center_axis',(0.,0.,-1.));
#7859=DIRECTION('ref_axis',(1.,-1.81324693622859E-14,0.));
#7860=DIRECTION('center_axis',(0.,0.,-1.));
#7861=DIRECTION('ref_axis',(1.,-2.31183580855735E-14,0.));
#7862=DIRECTION('center_axis',(0.,0.,-1.));
#7863=DIRECTION('ref_axis',(1.,0.,0.));
#7864=DIRECTION('center_axis',(0.,0.,-1.));
#7865=DIRECTION('ref_axis',(1.,0.,0.));
#7866=DIRECTION('center_axis',(0.,0.,-1.));
#7867=DIRECTION('ref_axis',(1.,0.,0.));
#7868=DIRECTION('center_axis',(0.,0.,-1.));
#7869=DIRECTION('ref_axis',(1.,0.,0.));
#7870=DIRECTION('center_axis',(0.,0.,-1.));
#7871=DIRECTION('ref_axis',(1.,0.,0.));
#7872=DIRECTION('center_axis',(0.,0.,-1.));
#7873=DIRECTION('ref_axis',(1.,0.,0.));
#7874=DIRECTION('',(0.,0.,-1.));
#7875=DIRECTION('center_axis',(0.,0.,1.));
#7876=DIRECTION('ref_axis',(1.,0.,0.));
#7877=DIRECTION('center_axis',(0.,0.,-1.));
#7878=DIRECTION('ref_axis',(1.,0.,0.));
#7879=DIRECTION('center_axis',(0.,0.,-1.));
#7880=DIRECTION('ref_axis',(1.,0.,0.));
#7881=DIRECTION('',(0.,0.,-1.));
#7882=DIRECTION('center_axis',(0.,0.,1.));
#7883=DIRECTION('ref_axis',(1.,0.,0.));
#7884=DIRECTION('center_axis',(0.,0.,-1.));
#7885=DIRECTION('ref_axis',(1.,0.,0.));
#7886=DIRECTION('center_axis',(0.,0.,-1.));
#7887=DIRECTION('ref_axis',(1.,0.,0.));
#7888=DIRECTION('',(0.,0.,-1.));
#7889=DIRECTION('center_axis',(0.,0.,1.));
#7890=DIRECTION('ref_axis',(1.,0.,0.));
#7891=DIRECTION('center_axis',(0.,0.,-1.));
#7892=DIRECTION('ref_axis',(1.,0.,0.));
#7893=DIRECTION('center_axis',(0.,0.,-1.));
#7894=DIRECTION('ref_axis',(1.,0.,0.));
#7895=DIRECTION('',(0.,0.,-1.));
#7896=DIRECTION('center_axis',(0.,0.,1.));
#7897=DIRECTION('ref_axis',(1.,0.,0.));
#7898=DIRECTION('center_axis',(0.,0.,1.));
#7899=DIRECTION('ref_axis',(1.,0.,0.));
#7900=DIRECTION('center_axis',(0.,0.,1.));
#7901=DIRECTION('ref_axis',(1.,0.,0.));
#7902=DIRECTION('center_axis',(0.,0.,1.));
#7903=DIRECTION('ref_axis',(1.,0.,0.));
#7904=DIRECTION('center_axis',(0.,0.,1.));
#7905=DIRECTION('ref_axis',(1.,0.,0.));
#7906=DIRECTION('',(0.,0.,-1.));
#7907=DIRECTION('center_axis',(0.,0.,1.));
#7908=DIRECTION('ref_axis',(1.,0.,0.));
#7909=DIRECTION('center_axis',(0.,0.,1.));
#7910=DIRECTION('ref_axis',(1.,0.,0.));
#7911=DIRECTION('center_axis',(0.,0.,-1.));
#7912=DIRECTION('ref_axis',(1.,0.,0.));
#7913=DIRECTION('center_axis',(0.,0.,1.));
#7914=DIRECTION('ref_axis',(1.,0.,0.));
#7915=DIRECTION('',(0.,0.,-1.));
#7916=DIRECTION('center_axis',(-0.866025403784438,0.5,0.));
#7917=DIRECTION('ref_axis',(-0.5,-0.866025403784438,0.));
#7918=DIRECTION('',(0.,0.,-1.));
#7919=DIRECTION('',(0.,0.,1.));
#7920=DIRECTION('',(-0.5,-0.866025403784438,0.));
#7921=DIRECTION('center_axis',(0.866025403784438,-0.5,0.));
#7922=DIRECTION('ref_axis',(0.5,0.866025403784438,0.));
#7923=DIRECTION('',(0.,0.,1.));
#7924=DIRECTION('',(0.5,0.866025403784438,0.));
#7925=DIRECTION('',(0.,0.,-1.));
#7926=DIRECTION('center_axis',(0.866025403784439,0.5,0.));
#7927=DIRECTION('ref_axis',(-0.5,0.866025403784439,0.));
#7928=DIRECTION('',(0.,0.,-1.));
#7929=DIRECTION('',(0.,0.,1.));
#7930=DIRECTION('',(-0.5,0.866025403784439,0.));
#7931=DIRECTION('center_axis',(-0.866025403784439,-0.5,0.));
#7932=DIRECTION('ref_axis',(0.5,-0.866025403784439,0.));
#7933=DIRECTION('',(0.,0.,1.));
#7934=DIRECTION('',(0.5,-0.866025403784439,0.));
#7935=DIRECTION('',(0.,0.,-1.));
#7936=DIRECTION('center_axis',(0.,0.,1.));
#7937=DIRECTION('ref_axis',(1.,0.,0.));
#7938=DIRECTION('',(0.,0.,-1.));
#7939=DIRECTION('center_axis',(0.,0.,-1.));
#7940=DIRECTION('ref_axis',(1.,0.,0.));
#7941=DIRECTION('',(0.,0.,1.));
#7942=DIRECTION('center_axis',(0.,0.,-1.));
#7943=DIRECTION('ref_axis',(1.,0.,0.));
#7944=DIRECTION('',(0.,0.,-1.));
#7945=DIRECTION('center_axis',(0.,0.,-1.));
#7946=DIRECTION('ref_axis',(1.,0.,0.));
#7947=DIRECTION('center_axis',(0.,0.,1.));
#7948=DIRECTION('ref_axis',(1.,0.,0.));
#7949=DIRECTION('',(1.,0.,0.));
#7950=DIRECTION('center_axis',(0.,0.,1.));
#7951=DIRECTION('ref_axis',(1.,0.,0.));
#7952=DIRECTION('center_axis',(0.,0.,1.));
#7953=DIRECTION('ref_axis',(1.,0.,0.));
#7954=DIRECTION('center_axis',(0.,0.,1.));
#7955=DIRECTION('ref_axis',(1.,0.,0.));
#7956=DIRECTION('',(-1.,0.,0.));
#7957=DIRECTION('center_axis',(0.,0.,-1.));
#7958=DIRECTION('ref_axis',(1.,0.,0.));
#7959=DIRECTION('center_axis',(0.,0.,1.));
#7960=DIRECTION('ref_axis',(1.,0.,0.));
#7961=DIRECTION('',(0.,0.,1.));
#7962=DIRECTION('center_axis',(0.,0.,1.));
#7963=DIRECTION('ref_axis',(-1.,-1.22464679914735E-16,0.));
#7964=DIRECTION('center_axis',(0.,0.,1.));
#7965=DIRECTION('ref_axis',(1.,0.,0.));
#7966=DIRECTION('',(0.,0.,-1.));
#7967=DIRECTION('center_axis',(0.,0.,1.));
#7968=DIRECTION('ref_axis',(1.,0.,0.));
#7969=DIRECTION('',(0.,0.,-1.));
#7970=DIRECTION('center_axis',(0.,1.,0.));
#7971=DIRECTION('ref_axis',(-1.,0.,0.));
#7972=DIRECTION('center_axis',(0.,0.,1.));
#7973=DIRECTION('ref_axis',(1.,0.,0.));
#7974=DIRECTION('center_axis',(0.,0.,1.));
#7975=DIRECTION('ref_axis',(1.,0.,0.));
#7976=DIRECTION('center_axis',(0.,-1.,0.));
#7977=DIRECTION('ref_axis',(1.,0.,0.));
#7978=DIRECTION('center_axis',(0.,0.,1.));
#7979=DIRECTION('ref_axis',(1.,0.,0.));
#7980=DIRECTION('',(0.,0.,-1.));
#7981=DIRECTION('axis',(0.,0.,1.));
#7982=DIRECTION('refdir',(1.,0.,0.));
#7983=DIRECTION('center_axis',(0.,1.,0.));
#7984=DIRECTION('ref_axis',(1.,0.,0.));
#7985=DIRECTION('center_axis',(0.,0.,1.));
#7986=DIRECTION('ref_axis',(1.,0.,0.));
#7987=DIRECTION('axis',(0.,0.,1.));
#7988=DIRECTION('refdir',(1.,0.,0.));
#7989=DIRECTION('center_axis',(0.707106781186548,0.707106781186548,0.));
#7990=DIRECTION('ref_axis',(-0.707106781186548,0.707106781186548,0.));
#7991=DIRECTION('center_axis',(0.707106781186548,0.707106781186548,0.));
#7992=DIRECTION('ref_axis',(-0.707106781186547,0.707106781186547,0.));
#7993=DIRECTION('center_axis',(-0.707106781186548,-0.707106781186548,0.));
#7994=DIRECTION('ref_axis',(-0.707106781186547,0.707106781186547,0.));
#7995=DIRECTION('center_axis',(-0.707106781186548,-0.707106781186548,0.));
#7996=DIRECTION('ref_axis',(-0.707106781186547,0.707106781186547,0.));
#7997=DIRECTION('center_axis',(-0.707106781186548,-0.707106781186548,0.));
#7998=DIRECTION('ref_axis',(-0.707106781186547,0.707106781186547,0.));
#7999=DIRECTION('center_axis',(-0.707106781186548,-0.707106781186548,0.));
#8000=DIRECTION('ref_axis',(-0.707106781186548,0.707106781186548,0.));
#8001=DIRECTION('center_axis',(-0.707106781186548,-0.707106781186548,0.));
#8002=DIRECTION('ref_axis',(-0.707106781186547,0.707106781186547,0.));
#8003=DIRECTION('center_axis',(-0.707106781186548,-0.707106781186548,0.));
#8004=DIRECTION('ref_axis',(0.,0.,1.));
#8005=DIRECTION('',(-0.707106781186548,-0.707106781186548,0.));
#8006=DIRECTION('center_axis',(0.707106781186548,0.707106781186548,0.));
#8007=DIRECTION('ref_axis',(0.,0.,1.));
#8008=DIRECTION('center_axis',(-0.707106781186548,-0.707106781186548,0.));
#8009=DIRECTION('ref_axis',(0.,0.,1.));
#8010=DIRECTION('',(-0.707106781186548,-0.707106781186548,0.));
#8011=DIRECTION('center_axis',(0.707106781186548,0.707106781186548,0.));
#8012=DIRECTION('ref_axis',(0.,0.,1.));
#8013=DIRECTION('center_axis',(-0.707106781186548,-0.707106781186548,0.));
#8014=DIRECTION('ref_axis',(0.,0.,1.));
#8015=DIRECTION('',(-0.707106781186548,-0.707106781186548,0.));
#8016=DIRECTION('center_axis',(0.707106781186548,0.707106781186548,0.));
#8017=DIRECTION('ref_axis',(0.,0.,1.));
#8018=DIRECTION('center_axis',(-0.707106781186548,-0.707106781186547,3.92523114670943E-17));
#8019=DIRECTION('ref_axis',(-0.707106781186547,0.707106781186548,0.));
#8020=DIRECTION('',(-0.707106781186548,-0.707106781186547,3.92523114670943E-17));
#8021=DIRECTION('center_axis',(0.707106781186548,0.707106781186548,0.));
#8022=DIRECTION('ref_axis',(-0.707106781186547,0.707106781186548,0.));
#8023=DIRECTION('center_axis',(0.707106781186548,0.707106781186548,0.));
#8024=DIRECTION('ref_axis',(0.,0.,1.));
#8025=DIRECTION('center_axis',(0.707106781186548,0.707106781186548,0.));
#8026=DIRECTION('ref_axis',(0.,0.,1.));
#8027=DIRECTION('center_axis',(0.707106781186548,0.707106781186548,0.));
#8028=DIRECTION('ref_axis',(0.,0.,1.));
#8029=DIRECTION('center_axis',(0.707106781186548,0.707106781186548,0.));
#8030=DIRECTION('ref_axis',(0.,0.,1.));
#8031=DIRECTION('',(-0.707106781186548,-0.707106781186548,0.));
#8032=DIRECTION('center_axis',(0.707106781186548,0.707106781186548,0.));
#8033=DIRECTION('ref_axis',(0.,0.,1.));
#8034=DIRECTION('',(0.707106781186548,-0.707106781186548,0.));
#8035=DIRECTION('center_axis',(0.707106781186548,0.707106781186548,0.));
#8036=DIRECTION('ref_axis',(0.,0.,1.));
#8037=DIRECTION('center_axis',(-0.707106781186548,-0.707106781186548,0.));
#8038=DIRECTION('ref_axis',(0.,0.,1.));
#8039=DIRECTION('center_axis',(0.707106781186548,0.707106781186548,0.));
#8040=DIRECTION('ref_axis',(0.,0.,1.));
#8041=DIRECTION('',(-0.707106781186548,-0.707106781186548,0.));
#8042=DIRECTION('center_axis',(0.707106781186548,0.707106781186548,0.));
#8043=DIRECTION('ref_axis',(0.,0.,1.));
#8044=DIRECTION('',(-0.707106781186548,-0.707106781186548,0.));
#8045=DIRECTION('center_axis',(0.707106781186548,0.707106781186548,0.));
#8046=DIRECTION('ref_axis',(8.65956056235493E-17,-8.65956056235493E-17,
-1.));
#8047=DIRECTION('',(0.707106781186548,0.707106781186548,0.));
#8048=DIRECTION('',(-0.707106781186548,-0.707106781186548,0.));
#8049=DIRECTION('center_axis',(0.,0.,1.));
#8050=DIRECTION('ref_axis',(1.,0.,0.));
#8051=DIRECTION('center_axis',(0.,0.,-1.));
#8052=DIRECTION('ref_axis',(1.,0.,0.));
#8053=DIRECTION('',(0.,0.,-1.));
#8054=DIRECTION('center_axis',(0.,0.,-1.));
#8055=DIRECTION('ref_axis',(1.,0.,0.));
#8056=DIRECTION('center_axis',(0.,0.,-1.));
#8057=DIRECTION('ref_axis',(1.,0.,0.));
#8058=DIRECTION('center_axis',(0.,0.,1.));
#8059=DIRECTION('ref_axis',(1.,0.,0.));
#8060=DIRECTION('center_axis',(0.,0.,1.));
#8061=DIRECTION('ref_axis',(1.,0.,0.));
#8062=DIRECTION('',(0.,0.,-1.));
#8063=DIRECTION('center_axis',(0.,0.,1.));
#8064=DIRECTION('ref_axis',(1.,0.,0.));
#8065=DIRECTION('center_axis',(0.,0.,-1.));
#8066=DIRECTION('ref_axis',(1.,0.,0.));
#8067=DIRECTION('center_axis',(0.,0.,-1.));
#8068=DIRECTION('ref_axis',(1.,0.,0.));
#8069=DIRECTION('',(0.,0.,-1.));
#8070=DIRECTION('center_axis',(0.,0.,1.));
#8071=DIRECTION('ref_axis',(1.,0.,0.));
#8072=DIRECTION('center_axis',(0.,0.,-1.));
#8073=DIRECTION('ref_axis',(1.,0.,0.));
#8074=DIRECTION('center_axis',(0.,0.,-1.));
#8075=DIRECTION('ref_axis',(1.,0.,0.));
#8076=DIRECTION('',(0.,0.,-1.));
#8077=DIRECTION('center_axis',(0.,0.,1.));
#8078=DIRECTION('ref_axis',(1.,0.,0.));
#8079=DIRECTION('center_axis',(0.,0.,-1.));
#8080=DIRECTION('ref_axis',(1.,0.,0.));
#8081=DIRECTION('center_axis',(0.,0.,-1.));
#8082=DIRECTION('ref_axis',(1.,0.,0.));
#8083=DIRECTION('',(0.,0.,-1.));
#8084=DIRECTION('center_axis',(0.,0.,1.));
#8085=DIRECTION('ref_axis',(1.,0.,0.));
#8086=DIRECTION('center_axis',(0.,0.,-1.));
#8087=DIRECTION('ref_axis',(1.,0.,0.));
#8088=DIRECTION('center_axis',(0.,0.,-1.));
#8089=DIRECTION('ref_axis',(1.,0.,0.));
#8090=DIRECTION('',(0.,0.,-1.));
#8091=DIRECTION('center_axis',(0.,0.,1.));
#8092=DIRECTION('ref_axis',(1.,0.,0.));
#8093=DIRECTION('center_axis',(0.,0.,1.));
#8094=DIRECTION('ref_axis',(1.,0.,0.));
#8095=DIRECTION('center_axis',(0.,0.,-1.));
#8096=DIRECTION('ref_axis',(1.,0.,0.));
#8097=DIRECTION('',(0.,0.,-1.));
#8098=DIRECTION('center_axis',(0.,0.,-1.));
#8099=DIRECTION('ref_axis',(1.,0.,0.));
#8100=DIRECTION('center_axis',(0.,0.,1.));
#8101=DIRECTION('ref_axis',(1.,0.,0.));
#8102=DIRECTION('center_axis',(0.,0.,1.));
#8103=DIRECTION('ref_axis',(1.,0.,0.));
#8104=DIRECTION('center_axis',(0.,0.,1.));
#8105=DIRECTION('ref_axis',(1.,0.,0.));
#8106=DIRECTION('center_axis',(0.,0.,-1.));
#8107=DIRECTION('ref_axis',(1.,0.,0.));
#8108=DIRECTION('center_axis',(0.,0.,-1.));
#8109=DIRECTION('ref_axis',(1.,0.,0.));
#8110=DIRECTION('center_axis',(0.,0.,1.));
#8111=DIRECTION('ref_axis',(1.,0.,0.));
#8112=DIRECTION('',(0.,0.,-1.));
#8113=DIRECTION('center_axis',(0.,0.,-1.));
#8114=DIRECTION('ref_axis',(1.,0.,0.));
#8115=DIRECTION('center_axis',(0.,0.,1.));
#8116=DIRECTION('ref_axis',(1.,0.,0.));
#8117=DIRECTION('center_axis',(0.,0.,1.));
#8118=DIRECTION('ref_axis',(1.,0.,0.));
#8119=DIRECTION('',(0.,0.,-1.));
#8120=DIRECTION('center_axis',(0.,0.,1.));
#8121=DIRECTION('ref_axis',(1.,0.,0.));
#8122=DIRECTION('center_axis',(0.,0.,1.));
#8123=DIRECTION('ref_axis',(1.,0.,0.));
#8124=DIRECTION('center_axis',(0.,0.,1.));
#8125=DIRECTION('ref_axis',(1.,0.,0.));
#8126=DIRECTION('center_axis',(0.,0.,-1.));
#8127=DIRECTION('ref_axis',(1.,0.,0.));
#8128=DIRECTION('',(0.,0.,-1.));
#8129=DIRECTION('center_axis',(0.,0.,1.));
#8130=DIRECTION('ref_axis',(1.,0.,0.));
#8131=DIRECTION('center_axis',(0.,0.,1.));
#8132=DIRECTION('ref_axis',(1.,0.,0.));
#8133=DIRECTION('axis',(0.,0.,1.));
#8134=DIRECTION('refdir',(1.,0.,0.));
#8135=DIRECTION('center_axis',(1.,0.,0.));
#8136=DIRECTION('ref_axis',(0.,1.,5.9211894646675E-15));
#8137=DIRECTION('',(1.,0.,0.));
#8138=DIRECTION('center_axis',(1.,0.,0.));
#8139=DIRECTION('ref_axis',(0.,1.,5.9211894646675E-15));
#8140=DIRECTION('',(1.,0.,0.));
#8141=DIRECTION('center_axis',(1.,0.,0.));
#8142=DIRECTION('ref_axis',(0.,1.,5.9211894646675E-15));
#8143=DIRECTION('',(1.,0.,0.));
#8144=DIRECTION('center_axis',(1.,0.,0.));
#8145=DIRECTION('ref_axis',(0.,1.,5.9211894646675E-15));
#8146=DIRECTION('',(1.,0.,0.));
#8147=DIRECTION('center_axis',(0.,1.,0.));
#8148=DIRECTION('ref_axis',(0.,0.,1.));
#8149=DIRECTION('',(0.,0.,-1.));
#8150=DIRECTION('',(0.,0.,-1.));
#8151=DIRECTION('',(1.,0.,0.));
#8152=DIRECTION('center_axis',(1.,0.,0.));
#8153=DIRECTION('ref_axis',(0.,-1.,-5.9211894646675E-15));
#8154=DIRECTION('center_axis',(1.,0.,0.));
#8155=DIRECTION('ref_axis',(0.,-1.,-5.9211894646675E-15));
#8156=DIRECTION('',(1.,0.,0.));
#8157=DIRECTION('center_axis',(0.,-1.,0.));
#8158=DIRECTION('ref_axis',(0.,0.,-1.));
#8159=DIRECTION('',(0.,0.,1.));
#8160=DIRECTION('',(0.,0.,1.));
#8161=DIRECTION('center_axis',(1.,0.,0.));
#8162=DIRECTION('ref_axis',(0.,0.,-1.));
#8163=DIRECTION('center_axis',(0.,0.,1.));
#8164=DIRECTION('ref_axis',(1.,0.,0.));
#8165=DIRECTION('center_axis',(0.,0.,1.));
#8166=DIRECTION('ref_axis',(1.,0.,0.));
#8167=DIRECTION('center_axis',(0.,0.,1.));
#8168=DIRECTION('ref_axis',(1.,0.,0.));
#8169=DIRECTION('',(0.,0.,-1.));
#8170=DIRECTION('center_axis',(0.,0.,1.));
#8171=DIRECTION('ref_axis',(1.,0.,0.));
#8172=DIRECTION('center_axis',(0.,-1.,0.));
#8173=DIRECTION('ref_axis',(0.,0.,-1.));
#8174=DIRECTION('',(0.,0.,1.));
#8175=DIRECTION('',(1.,0.,0.));
#8176=DIRECTION('',(0.,0.,1.));
#8177=DIRECTION('',(1.,0.,0.));
#8178=DIRECTION('center_axis',(1.,0.,0.));
#8179=DIRECTION('ref_axis',(0.,1.,0.));
#8180=DIRECTION('center_axis',(1.,0.,0.));
#8181=DIRECTION('ref_axis',(0.,1.,0.));
#8182=DIRECTION('',(1.,0.,0.));
#8183=DIRECTION('center_axis',(0.,1.,0.));
#8184=DIRECTION('ref_axis',(0.,0.,1.));
#8185=DIRECTION('',(0.,0.,-1.));
#8186=DIRECTION('',(0.,0.,-1.));
#8187=DIRECTION('',(1.,0.,0.));
#8188=DIRECTION('center_axis',(1.,0.,0.));
#8189=DIRECTION('ref_axis',(0.,-1.,-2.96059473233375E-15));
#8190=DIRECTION('center_axis',(1.,0.,0.));
#8191=DIRECTION('ref_axis',(0.,-1.,-2.96059473233375E-15));
#8192=DIRECTION('center_axis',(1.,0.,0.));
#8193=DIRECTION('ref_axis',(0.,0.,-1.));
#8194=DIRECTION('center_axis',(0.,-1.,0.));
#8195=DIRECTION('ref_axis',(0.,0.,-1.));
#8196=DIRECTION('',(0.,0.,1.));
#8197=DIRECTION('',(1.,0.,0.));
#8198=DIRECTION('',(0.,0.,1.));
#8199=DIRECTION('',(1.,0.,0.));
#8200=DIRECTION('center_axis',(1.,0.,0.));
#8201=DIRECTION('ref_axis',(0.,1.,0.));
#8202=DIRECTION('center_axis',(1.,0.,0.));
#8203=DIRECTION('ref_axis',(0.,1.,0.));
#8204=DIRECTION('',(1.,0.,0.));
#8205=DIRECTION('center_axis',(0.,1.,0.));
#8206=DIRECTION('ref_axis',(0.,0.,1.));
#8207=DIRECTION('',(0.,0.,-1.));
#8208=DIRECTION('',(0.,0.,-1.));
#8209=DIRECTION('',(1.,0.,0.));
#8210=DIRECTION('center_axis',(1.,0.,0.));
#8211=DIRECTION('ref_axis',(0.,-1.,0.));
#8212=DIRECTION('center_axis',(1.,0.,0.));
#8213=DIRECTION('ref_axis',(0.,-1.,0.));
#8214=DIRECTION('center_axis',(1.,0.,0.));
#8215=DIRECTION('ref_axis',(0.,0.,-1.));
#8216=DIRECTION('center_axis',(0.,0.,1.));
#8217=DIRECTION('ref_axis',(1.,0.,0.));
#8218=DIRECTION('center_axis',(0.,0.,1.));
#8219=DIRECTION('ref_axis',(1.,0.,0.));
#8220=DIRECTION('',(0.,0.,1.));
#8221=DIRECTION('center_axis',(0.,0.,1.));
#8222=DIRECTION('ref_axis',(1.,0.,0.));
#8223=DIRECTION('center_axis',(0.,0.,-1.));
#8224=DIRECTION('ref_axis',(-1.,0.,0.));
#8225=DIRECTION('center_axis',(0.,0.,-1.));
#8226=DIRECTION('ref_axis',(1.,0.,0.));
#8227=DIRECTION('center_axis',(0.,0.,1.));
#8228=DIRECTION('ref_axis',(1.,0.,0.));
#8229=DIRECTION('center_axis',(0.,0.,1.));
#8230=DIRECTION('ref_axis',(1.,0.,0.));
#8231=DIRECTION('center_axis',(0.,0.,1.));
#8232=DIRECTION('ref_axis',(1.,0.,0.));
#8233=DIRECTION('center_axis',(0.,0.,1.));
#8234=DIRECTION('ref_axis',(1.,0.,0.));
#8235=DIRECTION('center_axis',(0.,0.,1.));
#8236=DIRECTION('ref_axis',(1.,0.,0.));
#8237=DIRECTION('center_axis',(0.,0.,1.));
#8238=DIRECTION('ref_axis',(1.,0.,0.));
#8239=DIRECTION('center_axis',(0.,0.,-1.));
#8240=DIRECTION('ref_axis',(1.,0.,0.));
#8241=DIRECTION('center_axis',(0.,0.,1.));
#8242=DIRECTION('ref_axis',(1.,0.,0.));
#8243=DIRECTION('',(0.,0.,-1.));
#8244=DIRECTION('center_axis',(0.,0.,1.));
#8245=DIRECTION('ref_axis',(1.,0.,0.));
#8246=DIRECTION('',(0.,0.,-1.));
#8247=DIRECTION('center_axis',(0.,0.,1.));
#8248=DIRECTION('ref_axis',(1.,0.,0.));
#8249=DIRECTION('center_axis',(0.,0.,1.));
#8250=DIRECTION('ref_axis',(1.,0.,0.));
#8251=DIRECTION('',(0.,0.,-1.));
#8252=DIRECTION('center_axis',(0.,0.,1.));
#8253=DIRECTION('ref_axis',(1.,0.,0.));
#8254=DIRECTION('center_axis',(0.,0.,1.));
#8255=DIRECTION('ref_axis',(1.,0.,0.));
#8256=DIRECTION('axis',(0.,0.,1.));
#8257=DIRECTION('refdir',(1.,0.,0.));
#8258=DIRECTION('center_axis',(0.,0.,1.));
#8259=DIRECTION('ref_axis',(1.,0.,0.));
#8260=DIRECTION('center_axis',(0.,0.,-1.));
#8261=DIRECTION('ref_axis',(1.,0.,0.));
#8262=DIRECTION('',(0.,0.,-1.));
#8263=DIRECTION('center_axis',(0.,0.,-1.));
#8264=DIRECTION('ref_axis',(1.,0.,0.));
#8265=DIRECTION('center_axis',(0.,0.,1.));
#8266=DIRECTION('ref_axis',(1.,0.,0.));
#8267=DIRECTION('center_axis',(0.,0.,1.));
#8268=DIRECTION('ref_axis',(1.,0.,0.));
#8269=DIRECTION('',(0.,0.,-1.));
#8270=DIRECTION('center_axis',(0.,0.,1.));
#8271=DIRECTION('ref_axis',(1.,0.,0.));
#8272=DIRECTION('center_axis',(0.,0.,1.));
#8273=DIRECTION('ref_axis',(1.,0.,0.));
#8274=DIRECTION('center_axis',(0.,0.,1.));
#8275=DIRECTION('ref_axis',(1.,0.,0.));
#8276=DIRECTION('axis',(0.,0.,1.));
#8277=DIRECTION('refdir',(1.,0.,0.));
#8278=DIRECTION('center_axis',(0.,0.,1.));
#8279=DIRECTION('ref_axis',(1.,0.,0.));
#8280=DIRECTION('center_axis',(0.,0.,-1.));
#8281=DIRECTION('ref_axis',(1.,0.,0.));
#8282=DIRECTION('',(0.,0.,-1.));
#8283=DIRECTION('center_axis',(0.,0.,-1.));
#8284=DIRECTION('ref_axis',(1.,0.,0.));
#8285=DIRECTION('center_axis',(0.,0.,1.));
#8286=DIRECTION('ref_axis',(1.,0.,0.));
#8287=DIRECTION('center_axis',(0.,0.,1.));
#8288=DIRECTION('ref_axis',(1.,0.,0.));
#8289=DIRECTION('',(0.,0.,-1.));
#8290=DIRECTION('center_axis',(0.,0.,1.));
#8291=DIRECTION('ref_axis',(1.,0.,0.));
#8292=DIRECTION('center_axis',(0.,0.,1.));
#8293=DIRECTION('ref_axis',(1.,0.,0.));
#8294=DIRECTION('center_axis',(0.,0.,1.));
#8295=DIRECTION('ref_axis',(1.,0.,0.));
#8296=DIRECTION('axis',(0.,0.,1.));
#8297=DIRECTION('refdir',(1.,0.,0.));
#8298=DIRECTION('center_axis',(0.,0.,1.));
#8299=DIRECTION('ref_axis',(1.,0.,0.));
#8300=DIRECTION('center_axis',(0.,0.,-1.));
#8301=DIRECTION('ref_axis',(1.,0.,0.));
#8302=DIRECTION('',(0.,0.,-1.));
#8303=DIRECTION('center_axis',(0.,0.,-1.));
#8304=DIRECTION('ref_axis',(1.,0.,0.));
#8305=DIRECTION('center_axis',(0.,0.,1.));
#8306=DIRECTION('ref_axis',(1.,0.,0.));
#8307=DIRECTION('center_axis',(0.,0.,1.));
#8308=DIRECTION('ref_axis',(1.,0.,0.));
#8309=DIRECTION('',(0.,0.,-1.));
#8310=DIRECTION('center_axis',(0.,0.,1.));
#8311=DIRECTION('ref_axis',(1.,0.,0.));
#8312=DIRECTION('center_axis',(0.,0.,1.));
#8313=DIRECTION('ref_axis',(1.,0.,0.));
#8314=DIRECTION('center_axis',(0.,0.,1.));
#8315=DIRECTION('ref_axis',(1.,0.,0.));
#8316=DIRECTION('axis',(0.,0.,1.));
#8317=DIRECTION('refdir',(1.,0.,0.));
#8318=DIRECTION('center_axis',(0.,0.,1.));
#8319=DIRECTION('ref_axis',(1.,0.,0.));
#8320=DIRECTION('center_axis',(0.,0.,-1.));
#8321=DIRECTION('ref_axis',(1.,0.,0.));
#8322=DIRECTION('',(0.,0.,-1.));
#8323=DIRECTION('center_axis',(0.,0.,-1.));
#8324=DIRECTION('ref_axis',(1.,0.,0.));
#8325=DIRECTION('center_axis',(0.,0.,1.));
#8326=DIRECTION('ref_axis',(1.,0.,0.));
#8327=DIRECTION('center_axis',(0.,0.,1.));
#8328=DIRECTION('ref_axis',(1.,0.,0.));
#8329=DIRECTION('',(0.,0.,-1.));
#8330=DIRECTION('center_axis',(0.,0.,1.));
#8331=DIRECTION('ref_axis',(1.,0.,0.));
#8332=DIRECTION('center_axis',(0.,0.,1.));
#8333=DIRECTION('ref_axis',(1.,0.,0.));
#8334=DIRECTION('center_axis',(0.,0.,1.));
#8335=DIRECTION('ref_axis',(1.,0.,0.));
#8336=DIRECTION('axis',(0.,0.,1.));
#8337=DIRECTION('refdir',(1.,0.,0.));
#8338=DIRECTION('center_axis',(0.,1.,0.));
#8339=DIRECTION('ref_axis',(0.,0.,1.));
#8340=DIRECTION('',(0.,0.,-1.));
#8341=DIRECTION('',(1.,0.,0.));
#8342=DIRECTION('',(0.,0.,1.));
#8343=DIRECTION('',(1.,0.,0.));
#8344=DIRECTION('center_axis',(1.,0.,0.));
#8345=DIRECTION('ref_axis',(0.,-1.,0.));
#8346=DIRECTION('center_axis',(1.,0.,0.));
#8347=DIRECTION('ref_axis',(0.,-1.,0.));
#8348=DIRECTION('center_axis',(1.,0.,0.));
#8349=DIRECTION('ref_axis',(0.,-1.,0.));
#8350=DIRECTION('',(1.,0.,0.));
#8351=DIRECTION('center_axis',(0.,-1.,0.));
#8352=DIRECTION('ref_axis',(0.,0.,-1.));
#8353=DIRECTION('',(0.,0.,1.));
#8354=DIRECTION('',(0.,0.,-1.));
#8355=DIRECTION('',(1.,0.,0.));
#8356=DIRECTION('center_axis',(1.,0.,0.));
#8357=DIRECTION('ref_axis',(0.,1.,0.));
#8358=DIRECTION('center_axis',(1.,0.,0.));
#8359=DIRECTION('ref_axis',(0.,1.,0.));
#8360=DIRECTION('center_axis',(1.,0.,0.));
#8361=DIRECTION('ref_axis',(0.,1.,0.));
#8362=DIRECTION('center_axis',(1.,0.,0.));
#8363=DIRECTION('ref_axis',(0.,0.,-1.));
#8364=DIRECTION('center_axis',(1.,0.,0.));
#8365=DIRECTION('ref_axis',(0.,0.,-1.));
#8366=DIRECTION('axis',(0.,0.,1.));
#8367=DIRECTION('refdir',(1.,0.,0.));
#8368=DIRECTION('center_axis',(0.,0.,1.));
#8369=DIRECTION('ref_axis',(1.,0.,0.));
#8370=DIRECTION('center_axis',(0.,0.,-1.));
#8371=DIRECTION('ref_axis',(1.,0.,0.));
#8372=DIRECTION('',(0.,0.,-1.));
#8373=DIRECTION('center_axis',(0.,0.,-1.));
#8374=DIRECTION('ref_axis',(1.,0.,0.));
#8375=DIRECTION('center_axis',(0.,0.,1.));
#8376=DIRECTION('ref_axis',(1.,0.,0.));
#8377=DIRECTION('center_axis',(0.,0.,1.));
#8378=DIRECTION('ref_axis',(1.,0.,0.));
#8379=DIRECTION('',(0.,0.,-1.));
#8380=DIRECTION('center_axis',(0.,0.,1.));
#8381=DIRECTION('ref_axis',(1.,0.,0.));
#8382=DIRECTION('center_axis',(0.,0.,1.));
#8383=DIRECTION('ref_axis',(1.,0.,0.));
#8384=DIRECTION('center_axis',(0.,0.,1.));
#8385=DIRECTION('ref_axis',(1.,0.,0.));
#8386=DIRECTION('axis',(0.,0.,1.));
#8387=DIRECTION('refdir',(1.,0.,0.));
#8388=DIRECTION('center_axis',(0.,0.,1.));
#8389=DIRECTION('ref_axis',(1.,0.,0.));
#8390=DIRECTION('center_axis',(0.,0.,-1.));
#8391=DIRECTION('ref_axis',(1.,0.,0.));
#8392=DIRECTION('',(0.,0.,-1.));
#8393=DIRECTION('center_axis',(0.,0.,-1.));
#8394=DIRECTION('ref_axis',(1.,0.,0.));
#8395=DIRECTION('center_axis',(0.,0.,1.));
#8396=DIRECTION('ref_axis',(1.,0.,0.));
#8397=DIRECTION('center_axis',(0.,0.,1.));
#8398=DIRECTION('ref_axis',(1.,0.,0.));
#8399=DIRECTION('',(0.,0.,-1.));
#8400=DIRECTION('center_axis',(0.,0.,1.));
#8401=DIRECTION('ref_axis',(1.,0.,0.));
#8402=DIRECTION('center_axis',(0.,0.,1.));
#8403=DIRECTION('ref_axis',(1.,0.,0.));
#8404=DIRECTION('center_axis',(0.,0.,1.));
#8405=DIRECTION('ref_axis',(1.,0.,0.));
#8406=DIRECTION('axis',(0.,0.,1.));
#8407=DIRECTION('refdir',(1.,0.,0.));
#8408=DIRECTION('center_axis',(0.,0.,1.));
#8409=DIRECTION('ref_axis',(1.,0.,0.));
#8410=DIRECTION('center_axis',(0.,0.,-1.));
#8411=DIRECTION('ref_axis',(1.,0.,0.));
#8412=DIRECTION('',(0.,0.,-1.));
#8413=DIRECTION('center_axis',(0.,0.,-1.));
#8414=DIRECTION('ref_axis',(1.,0.,0.));
#8415=DIRECTION('center_axis',(0.,0.,1.));
#8416=DIRECTION('ref_axis',(1.,0.,0.));
#8417=DIRECTION('center_axis',(0.,0.,1.));
#8418=DIRECTION('ref_axis',(1.,0.,0.));
#8419=DIRECTION('',(0.,0.,-1.));
#8420=DIRECTION('center_axis',(0.,0.,1.));
#8421=DIRECTION('ref_axis',(1.,0.,0.));
#8422=DIRECTION('center_axis',(0.,0.,1.));
#8423=DIRECTION('ref_axis',(1.,0.,0.));
#8424=DIRECTION('center_axis',(0.,0.,1.));
#8425=DIRECTION('ref_axis',(1.,0.,0.));
#8426=DIRECTION('axis',(0.,0.,1.));
#8427=DIRECTION('refdir',(1.,0.,0.));
#8428=DIRECTION('center_axis',(0.,0.,1.));
#8429=DIRECTION('ref_axis',(1.,0.,0.));
#8430=DIRECTION('center_axis',(0.,0.,-1.));
#8431=DIRECTION('ref_axis',(1.,0.,0.));
#8432=DIRECTION('',(0.,0.,-1.));
#8433=DIRECTION('center_axis',(0.,0.,-1.));
#8434=DIRECTION('ref_axis',(1.,0.,0.));
#8435=DIRECTION('center_axis',(0.,0.,1.));
#8436=DIRECTION('ref_axis',(1.,0.,0.));
#8437=DIRECTION('center_axis',(0.,0.,1.));
#8438=DIRECTION('ref_axis',(1.,0.,0.));
#8439=DIRECTION('',(0.,0.,-1.));
#8440=DIRECTION('center_axis',(0.,0.,1.));
#8441=DIRECTION('ref_axis',(1.,0.,0.));
#8442=DIRECTION('center_axis',(0.,0.,1.));
#8443=DIRECTION('ref_axis',(1.,0.,0.));
#8444=DIRECTION('center_axis',(0.,0.,1.));
#8445=DIRECTION('ref_axis',(1.,0.,0.));
#8446=DIRECTION('axis',(0.,0.,1.));
#8447=DIRECTION('refdir',(1.,0.,0.));
#8448=DIRECTION('center_axis',(-1.,0.,0.));
#8449=DIRECTION('ref_axis',(0.,1.,0.));
#8450=DIRECTION('',(0.,0.,1.));
#8451=DIRECTION('',(0.,-1.,0.));
#8452=DIRECTION('',(0.,0.,-1.));
#8453=DIRECTION('',(0.,1.,0.));
#8454=DIRECTION('center_axis',(1.,0.,0.));
#8455=DIRECTION('ref_axis',(0.,-1.,0.));
#8456=DIRECTION('',(0.,0.,-1.));
#8457=DIRECTION('',(0.,-1.,0.));
#8458=DIRECTION('',(0.,0.,1.));
#8459=DIRECTION('',(0.,1.,0.));
#8460=DIRECTION('center_axis',(0.,0.,1.));
#8461=DIRECTION('ref_axis',(1.,0.,0.));
#8462=DIRECTION('center_axis',(0.,0.,1.));
#8463=DIRECTION('ref_axis',(1.,0.,0.));
#8464=DIRECTION('center_axis',(0.,0.,-1.));
#8465=DIRECTION('ref_axis',(1.,0.,0.));
#8466=DIRECTION('center_axis',(0.,0.,1.));
#8467=DIRECTION('ref_axis',(6.12323399573677E-17,-1.,0.));
#8468=DIRECTION('center_axis',(0.,0.,-1.));
#8469=DIRECTION('ref_axis',(1.,0.,0.));
#8470=DIRECTION('center_axis',(0.,0.,1.));
#8471=DIRECTION('ref_axis',(6.12323399573677E-17,-1.,0.));
#8472=DIRECTION('center_axis',(0.,0.,1.));
#8473=DIRECTION('ref_axis',(1.,0.,0.));
#8474=DIRECTION('center_axis',(0.,0.,1.));
#8475=DIRECTION('ref_axis',(1.,0.,0.));
#8476=DIRECTION('axis',(0.,0.,1.));
#8477=DIRECTION('refdir',(1.,0.,0.));
#8478=DIRECTION('center_axis',(0.,0.,1.));
#8479=DIRECTION('ref_axis',(1.,0.,0.));
#8480=DIRECTION('',(0.,0.,-1.));
#8481=DIRECTION('center_axis',(0.,0.,-1.));
#8482=DIRECTION('ref_axis',(1.,0.,0.));
#8483=DIRECTION('',(0.,0.,-1.));
#8484=DIRECTION('center_axis',(0.,0.,-1.));
#8485=DIRECTION('ref_axis',(1.,0.,0.));
#8486=DIRECTION('center_axis',(0.,0.,-1.));
#8487=DIRECTION('ref_axis',(1.,0.,0.));
#8488=DIRECTION('center_axis',(0.,0.,1.));
#8489=DIRECTION('ref_axis',(1.,0.,0.));
#8490=DIRECTION('',(0.,0.,-1.));
#8491=DIRECTION('center_axis',(0.,0.,1.));
#8492=DIRECTION('ref_axis',(1.,0.,0.));
#8493=DIRECTION('',(0.,0.,-1.));
#8494=DIRECTION('center_axis',(0.,0.,1.));
#8495=DIRECTION('ref_axis',(1.,0.,0.));
#8496=DIRECTION('',(0.,0.,-1.));
#8497=DIRECTION('center_axis',(0.,0.,1.));
#8498=DIRECTION('ref_axis',(1.,0.,0.));
#8499=DIRECTION('',(0.,0.,-1.));
#8500=DIRECTION('center_axis',(0.,0.,1.));
#8501=DIRECTION('ref_axis',(1.,0.,0.));
#8502=DIRECTION('',(0.,0.,-1.));
#8503=DIRECTION('center_axis',(0.,0.,1.));
#8504=DIRECTION('ref_axis',(1.,0.,0.));
#8505=DIRECTION('',(0.,0.,-1.));
#8506=DIRECTION('center_axis',(0.,0.,1.));
#8507=DIRECTION('ref_axis',(0.99733299283639,-0.0729856246120375,0.));
#8508=DIRECTION('',(0.,0.,1.));
#8509=DIRECTION('center_axis',(0.,0.,-1.));
#8510=DIRECTION('ref_axis',(1.,4.21694431476393E-14,0.));
#8511=DIRECTION('center_axis',(0.,0.,1.));
#8512=DIRECTION('ref_axis',(1.,4.21694431476393E-14,0.));
#8513=DIRECTION('',(0.,0.,1.));
#8514=DIRECTION('center_axis',(0.,0.,1.));
#8515=DIRECTION('ref_axis',(1.,4.21694431476393E-14,0.));
#8516=DIRECTION('',(0.,0.,1.));
#8517=DIRECTION('center_axis',(0.,0.,1.));
#8518=DIRECTION('ref_axis',(1.,4.21694431476393E-14,0.));
#8519=DIRECTION('',(0.,0.,1.));
#8520=DIRECTION('center_axis',(0.,0.,1.));
#8521=DIRECTION('ref_axis',(1.,4.21694431476393E-14,0.));
#8522=DIRECTION('',(0.,0.,1.));
#8523=DIRECTION('center_axis',(0.,0.,1.));
#8524=DIRECTION('ref_axis',(1.,4.21694431476393E-14,0.));
#8525=DIRECTION('',(0.,0.,1.));
#8526=DIRECTION('center_axis',(0.,0.,1.));
#8527=DIRECTION('ref_axis',(1.,4.21694431476393E-14,0.));
#8528=DIRECTION('',(0.,0.,1.));
#8529=DIRECTION('center_axis',(0.,0.,-1.));
#8530=DIRECTION('ref_axis',(1.,0.,0.));
#8531=DIRECTION('center_axis',(0.,0.,-1.));
#8532=DIRECTION('ref_axis',(1.,0.,0.));
#8533=DIRECTION('',(0.707106781186549,8.65956056235495E-17,0.707106781186546));
#8534=DIRECTION('center_axis',(0.,0.,1.));
#8535=DIRECTION('ref_axis',(1.,0.,0.));
#8536=DIRECTION('center_axis',(0.,0.,1.));
#8537=DIRECTION('ref_axis',(1.,4.21694431476393E-14,0.));
#8538=DIRECTION('center_axis',(0.,0.,-1.));
#8539=DIRECTION('ref_axis',(1.,4.21694431476393E-14,0.));
#8540=DIRECTION('center_axis',(0.,0.,1.));
#8541=DIRECTION('ref_axis',(1.,0.,0.));
#8542=DIRECTION('center_axis',(0.,0.,1.));
#8543=DIRECTION('ref_axis',(1.,0.,0.));
#8544=DIRECTION('center_axis',(-1.92296268638356E-16,-1.,0.));
#8545=DIRECTION('ref_axis',(1.,-1.92296268638356E-16,0.));
#8546=DIRECTION('',(1.,-1.92296268638356E-16,0.));
#8547=DIRECTION('',(0.,0.,1.));
#8548=DIRECTION('',(1.,-1.92296268638356E-16,0.));
#8549=DIRECTION('',(0.,0.,1.));
#8550=DIRECTION('center_axis',(-0.866025403784439,-0.5,0.));
#8551=DIRECTION('ref_axis',(0.5,-0.866025403784439,0.));
#8552=DIRECTION('',(0.5,-0.866025403784439,0.));
#8553=DIRECTION('',(0.,0.,1.));
#8554=DIRECTION('',(0.5,-0.866025403784439,0.));
#8555=DIRECTION('center_axis',(-0.866025403784439,0.5,0.));
#8556=DIRECTION('ref_axis',(-0.5,-0.866025403784439,0.));
#8557=DIRECTION('',(-0.5,-0.866025403784439,0.));
#8558=DIRECTION('',(0.,0.,1.));
#8559=DIRECTION('',(-0.5,-0.866025403784438,0.));
#8560=DIRECTION('center_axis',(1.92296268638356E-16,1.,0.));
#8561=DIRECTION('ref_axis',(-1.,1.92296268638356E-16,0.));
#8562=DIRECTION('',(-1.,1.92296268638356E-16,0.));
#8563=DIRECTION('',(0.,0.,1.));
#8564=DIRECTION('',(-1.,1.92296268638356E-16,0.));
#8565=DIRECTION('center_axis',(0.866025403784439,0.5,0.));
#8566=DIRECTION('ref_axis',(-0.5,0.866025403784439,0.));
#8567=DIRECTION('',(-0.5,0.866025403784439,0.));
#8568=DIRECTION('',(0.,0.,1.));
#8569=DIRECTION('',(-0.5,0.866025403784439,0.));
#8570=DIRECTION('center_axis',(0.866025403784439,-0.5,0.));
#8571=DIRECTION('ref_axis',(0.5,0.866025403784439,0.));
#8572=DIRECTION('',(0.5,0.866025403784439,0.));
#8573=DIRECTION('',(0.5,0.866025403784439,0.));
#8574=DIRECTION('center_axis',(0.,0.,1.));
#8575=DIRECTION('ref_axis',(1.,0.,0.));
#8576=DIRECTION('center_axis',(0.,0.,1.));
#8577=DIRECTION('ref_axis',(1.,0.,0.));
#8578=DIRECTION('center_axis',(0.,0.,1.));
#8579=DIRECTION('ref_axis',(1.,0.,0.));
#8580=DIRECTION('center_axis',(0.,0.,1.));
#8581=DIRECTION('ref_axis',(1.,0.,0.));
#8582=DIRECTION('',(0.,0.,-1.));
#8583=DIRECTION('center_axis',(0.,0.,1.));
#8584=DIRECTION('ref_axis',(1.,0.,0.));
#8585=DIRECTION('center_axis',(0.,0.,1.));
#8586=DIRECTION('ref_axis',(1.,0.,0.));
#8587=DIRECTION('center_axis',(0.,0.,1.));
#8588=DIRECTION('ref_axis',(1.,0.,0.));
#8589=DIRECTION('',(0.,0.,1.));
#8590=DIRECTION('',(1.,0.,0.));
#8591=DIRECTION('',(0.,0.,1.));
#8592=DIRECTION('',(1.,0.,0.));
#8593=DIRECTION('',(0.,0.,1.));
#8594=DIRECTION('',(0.738128650078755,0.674659985424447,0.));
#8595=DIRECTION('',(0.,0.,1.));
#8596=DIRECTION('',(1.,0.,0.));
#8597=DIRECTION('',(0.,0.,1.));
#8598=DIRECTION('',(1.,0.,0.));
#8599=DIRECTION('',(0.,0.,1.));
#8600=DIRECTION('',(1.,0.,0.));
#8601=DIRECTION('',(0.,0.,1.));
#8602=DIRECTION('',(0.738128650078755,0.674659985424447,0.));
#8603=DIRECTION('',(0.,0.,1.));
#8604=DIRECTION('',(1.,0.,0.));
#8605=DIRECTION('',(0.,0.,1.));
#8606=DIRECTION('',(1.,0.,0.));
#8607=DIRECTION('',(0.,0.,1.));
#8608=DIRECTION('',(1.,0.,0.));
#8609=DIRECTION('',(0.,0.,1.));
#8610=DIRECTION('',(1.,0.,0.));
#8611=DIRECTION('',(0.,0.,1.));
#8612=DIRECTION('',(1.,0.,0.));
#8613=DIRECTION('',(0.,0.,1.));
#8614=DIRECTION('',(1.,0.,0.));
#8615=DIRECTION('',(0.,0.,1.));
#8616=DIRECTION('',(1.,0.,0.));
#8617=DIRECTION('',(0.,0.,1.));
#8618=DIRECTION('',(1.,0.,0.));
#8619=DIRECTION('',(0.,0.,1.));
#8620=DIRECTION('',(0.738128650078755,0.674659985424447,0.));
#8621=DIRECTION('',(0.,0.,1.));
#8622=DIRECTION('',(0.738128650078755,0.674659985424447,0.));
#8623=DIRECTION('',(0.,0.,1.));
#8624=DIRECTION('',(0.738128650078755,0.674659985424447,0.));
#8625=DIRECTION('',(0.,0.,1.));
#8626=DIRECTION('',(0.738128650078755,0.674659985424447,0.));
#8627=DIRECTION('',(0.,0.,1.));
#8628=DIRECTION('',(0.738128650078755,0.674659985424447,0.));
#8629=DIRECTION('',(0.,0.,1.));
#8630=DIRECTION('',(1.,0.,0.));
#8631=DIRECTION('',(0.,0.,1.));
#8632=DIRECTION('',(0.738128650078755,0.674659985424447,0.));
#8633=DIRECTION('',(0.,0.,1.));
#8634=DIRECTION('',(1.,0.,0.));
#8635=DIRECTION('',(0.,0.,1.));
#8636=DIRECTION('',(0.738128650078755,0.674659985424447,0.));
#8637=DIRECTION('',(0.,0.,1.));
#8638=DIRECTION('',(1.,0.,0.));
#8639=DIRECTION('',(0.,0.,1.));
#8640=DIRECTION('',(0.738128650078755,0.674659985424447,0.));
#8641=DIRECTION('',(0.,0.,1.));
#8642=DIRECTION('',(0.738128650078755,0.674659985424447,0.));
#8643=DIRECTION('',(0.,-1.22464679914735E-16,-1.));
#8644=DIRECTION('',(1.,0.,0.));
#8645=DIRECTION('',(0.,-1.22464679914735E-16,-1.));
#8646=DIRECTION('',(1.,0.,0.));
#8647=DIRECTION('',(0.,-1.22464679914735E-16,-1.));
#8648=DIRECTION('',(1.,0.,0.));
#8649=DIRECTION('',(0.,-1.22464679914735E-16,-1.));
#8650=DIRECTION('',(1.,0.,0.));
#8651=CARTESIAN_POINT('',(0.,0.,0.));
#8652=CARTESIAN_POINT('',(0.,0.,0.));
#8653=CARTESIAN_POINT('Origin',(0.,0.,3.8));
#8654=CARTESIAN_POINT('',(-6.35,-7.77650717458569E-16,3.8));
#8655=CARTESIAN_POINT('Origin',(0.,0.,3.8));
#8656=CARTESIAN_POINT('',(-6.35,-7.77650717458569E-16,3.6));
#8657=CARTESIAN_POINT('',(-6.35,7.77650717458569E-16,3.8));
#8658=CARTESIAN_POINT('Origin',(0.,0.,3.6));
#8659=CARTESIAN_POINT('Origin',(0.,0.,3.8));
#8660=CARTESIAN_POINT('',(-6.85,-8.38883057415937E-16,3.8));
#8661=CARTESIAN_POINT('Origin',(0.,0.,3.8));
#8662=CARTESIAN_POINT('',(-6.85,-8.38883057415937E-16,3.6));
#8663=CARTESIAN_POINT('',(-6.85,8.38883057415937E-16,3.8));
#8664=CARTESIAN_POINT('Origin',(0.,0.,3.6));
#8665=CARTESIAN_POINT('Origin',(0.,0.,3.6));
#8666=CARTESIAN_POINT('Origin',(0.,0.,3.8));
#8667=CARTESIAN_POINT('',(-6.2,-7.59281015471359E-16,3.8));
#8668=CARTESIAN_POINT('Origin',(0.,0.,3.8));
#8669=CARTESIAN_POINT('Origin',(-7.4,0.,1.9));
#8670=CARTESIAN_POINT('',(-7.75,4.28626379701574E-17,3.8));
#8671=CARTESIAN_POINT('Origin',(-7.4,0.,3.8));
#8672=CARTESIAN_POINT('',(-7.75,4.28626379701574E-17,-2.22044604925031E-16));
#8673=CARTESIAN_POINT('',(-7.75,4.28626379701574E-17,1.9));
#8674=CARTESIAN_POINT('Origin',(-7.4,0.,0.));
#8675=CARTESIAN_POINT('Origin',(7.4,0.,1.9));
#8676=CARTESIAN_POINT('',(7.05,4.28626379701574E-17,3.8));
#8677=CARTESIAN_POINT('Origin',(7.4,0.,3.8));
#8678=CARTESIAN_POINT('',(7.05,4.28626379701574E-17,-2.22044604925031E-16));
#8679=CARTESIAN_POINT('',(7.05,4.28626379701574E-17,1.9));
#8680=CARTESIAN_POINT('Origin',(7.4,0.,0.));
#8681=CARTESIAN_POINT('Origin',(0.,7.4,1.9));
#8682=CARTESIAN_POINT('',(-0.35,7.4,3.8));
#8683=CARTESIAN_POINT('Origin',(0.,7.4,3.8));
#8684=CARTESIAN_POINT('',(-0.35,7.4,-2.22044604925031E-16));
#8685=CARTESIAN_POINT('',(-0.35,7.4,1.9));
#8686=CARTESIAN_POINT('Origin',(0.,7.4,0.));
#8687=CARTESIAN_POINT('Origin',(0.,-7.4,1.9));
#8688=CARTESIAN_POINT('',(-0.35,-7.4,3.8));
#8689=CARTESIAN_POINT('Origin',(0.,-7.4,3.8));
#8690=CARTESIAN_POINT('',(-0.35,-7.4,-2.22044604925031E-16));
#8691=CARTESIAN_POINT('',(-0.35,-7.4,1.9));
#8692=CARTESIAN_POINT('Origin',(0.,-7.4,0.));
#8693=CARTESIAN_POINT('Origin',(1.18660254037844,-1.85525588832577,3.2));
#8694=CARTESIAN_POINT('',(0.926794919243111,-2.00525588832577,3.2));
#8695=CARTESIAN_POINT('',(1.18660254037844,-1.85525588832577,3.2));
#8696=CARTESIAN_POINT('',(3.39330127018922,-0.58121778264911,3.2));
#8697=CARTESIAN_POINT('',(0.926794919243111,-2.00525588832577,3.8));
#8698=CARTESIAN_POINT('',(0.926794919243111,-2.00525588832577,3.2));
#8699=CARTESIAN_POINT('',(1.18660254037844,-1.85525588832577,3.8));
#8700=CARTESIAN_POINT('',(0.926794919243111,-2.00525588832577,3.8));
#8701=CARTESIAN_POINT('',(1.18660254037844,-1.85525588832577,3.2));
#8702=CARTESIAN_POINT('Origin',(3.69807621135331,-0.405255888325769,3.2));
#8703=CARTESIAN_POINT('',(3.39494366787712,-3.28936938489376,3.2));
#8704=CARTESIAN_POINT('Origin',(3.69807621135331,-0.405255888325769,3.2));
#8705=CARTESIAN_POINT('',(3.39494366787712,-3.28936938489376,3.8));
#8706=CARTESIAN_POINT('Origin',(3.69807621135331,-0.405255888325769,3.8));
#8707=CARTESIAN_POINT('',(3.39494366787712,-3.28936938489376,3.2));
#8708=CARTESIAN_POINT('Origin',(3.36358512889682,-3.58772595350424,3.2));
#8709=CARTESIAN_POINT('',(3.36358512889682,-3.58772595350424,3.2));
#8710=CARTESIAN_POINT('',(3.56447066879145,-1.6764277133635,3.2));
#8711=CARTESIAN_POINT('',(3.36358512889682,-3.58772595350424,3.8));
#8712=CARTESIAN_POINT('',(3.39494366787712,-3.28936938489376,3.8));
#8713=CARTESIAN_POINT('',(3.36358512889682,-3.58772595350424,3.2));
#8714=CARTESIAN_POINT('Origin',(3.69807621135331,-0.405255888325769,3.2));
#8715=CARTESIAN_POINT('Origin',(3.69807621135331,-0.405255888325769,3.2));
#8716=CARTESIAN_POINT('Origin',(3.69807621135331,-0.405255888325769,3.8));
#8717=CARTESIAN_POINT('Origin',(2.22154556813824,-2.75240702699307,3.8));
#8718=CARTESIAN_POINT('Origin',(-1.01339745962156,-1.95525588832576,3.2));
#8719=CARTESIAN_POINT('',(-1.27320508075689,-1.80525588832576,3.2));
#8720=CARTESIAN_POINT('',(-1.01339745962156,-1.95525588832576,3.2));
#8721=CARTESIAN_POINT('',(1.19330127018922,-3.22929399400242,3.2));
#8722=CARTESIAN_POINT('',(-1.27320508075689,-1.80525588832576,3.8));
#8723=CARTESIAN_POINT('',(-1.27320508075689,-1.80525588832576,3.2));
#8724=CARTESIAN_POINT('',(-1.01339745962156,-1.95525588832576,3.8));
#8725=CARTESIAN_POINT('',(-1.27320508075689,-1.80525588832576,3.8));
#8726=CARTESIAN_POINT('',(-1.01339745962156,-1.95525588832576,3.2));
#8727=CARTESIAN_POINT('Origin',(1.49807621135331,-3.40525588832577,3.2));
#8728=CARTESIAN_POINT('',(-1.15120561581023,-4.58479215324559,3.2));
#8729=CARTESIAN_POINT('Origin',(1.49807621135331,-3.40525588832577,3.2));
#8730=CARTESIAN_POINT('',(-1.15120561581023,-4.58479215324559,3.8));
#8731=CARTESIAN_POINT('Origin',(1.49807621135331,-3.40525588832577,3.8));
#8732=CARTESIAN_POINT('',(-1.15120561581023,-4.58479215324559,3.2));
#8733=CARTESIAN_POINT('Origin',(-1.42526925310301,-4.70681314616832,3.2));
#8734=CARTESIAN_POINT('',(-1.42526925310301,-4.70681314616832,3.2));
#8735=CARTESIAN_POINT('',(2.54762774811539,-2.93796543744964,3.2));
#8736=CARTESIAN_POINT('',(-1.42526925310301,-4.70681314616832,3.8));
#8737=CARTESIAN_POINT('',(-1.15120561581023,-4.58479215324559,3.8));
#8738=CARTESIAN_POINT('',(-1.42526925310301,-4.70681314616832,3.2));
#8739=CARTESIAN_POINT('Origin',(1.49807621135331,-3.40525588832577,3.2));
#8740=CARTESIAN_POINT('Origin',(1.49807621135331,-3.40525588832577,3.2));
#8741=CARTESIAN_POINT('Origin',(1.49807621135331,-3.40525588832577,3.8));
#8742=CARTESIAN_POINT('Origin',(-1.27288162286168,-3.30011841116898,3.8));
#8743=CARTESIAN_POINT('Origin',(-2.2,-0.0999999999999998,3.2));
#8744=CARTESIAN_POINT('',(-2.2,0.2,3.2));
#8745=CARTESIAN_POINT('',(-2.2,-0.0999999999999998,3.2));
#8746=CARTESIAN_POINT('',(-2.2,-0.0499999999999992,3.2));
#8747=CARTESIAN_POINT('',(-2.2,0.2,3.8));
#8748=CARTESIAN_POINT('',(-2.2,0.2,3.2));
#8749=CARTESIAN_POINT('',(-2.2,-0.0999999999999998,3.8));
#8750=CARTESIAN_POINT('',(-2.2,0.2,3.8));
#8751=CARTESIAN_POINT('',(-2.2,-0.0999999999999998,3.2));
#8752=CARTESIAN_POINT('Origin',(-2.2,-3.,3.2));
#8753=CARTESIAN_POINT('',(-4.54614928368735,-1.29542276835183,3.2));
#8754=CARTESIAN_POINT('Origin',(-2.2,-3.,3.2));
#8755=CARTESIAN_POINT('',(-4.54614928368735,-1.29542276835183,3.8));
#8756=CARTESIAN_POINT('Origin',(-2.2,-3.,3.8));
#8757=CARTESIAN_POINT('',(-4.54614928368735,-1.29542276835183,3.2));
#8758=CARTESIAN_POINT('Origin',(-4.78885438199983,-1.11908719266409,3.2));
#8759=CARTESIAN_POINT('',(-4.78885438199983,-1.11908719266409,3.2));
#8760=CARTESIAN_POINT('',(-1.52423473975264,-3.49097220051832,3.2));
#8761=CARTESIAN_POINT('',(-4.78885438199983,-1.11908719266409,3.8));
#8762=CARTESIAN_POINT('',(-4.54614928368735,-1.29542276835183,3.8));
#8763=CARTESIAN_POINT('',(-4.78885438199983,-1.11908719266409,3.2));
#8764=CARTESIAN_POINT('Origin',(-2.2,-3.,3.2));
#8765=CARTESIAN_POINT('Origin',(-2.2,-3.,3.2));
#8766=CARTESIAN_POINT('Origin',(-2.2,-3.,3.8));
#8767=CARTESIAN_POINT('Origin',(-3.49442719099992,-0.547711384175914,3.8));
#8768=CARTESIAN_POINT('Origin',(-1.18660254037844,1.85525588832577,3.2));
#8769=CARTESIAN_POINT('',(-0.926794919243112,2.00525588832577,3.2));
#8770=CARTESIAN_POINT('',(-1.18660254037844,1.85525588832577,3.2));
#8771=CARTESIAN_POINT('',(1.10669872981078,3.17929399400242,3.2));
#8772=CARTESIAN_POINT('',(-0.926794919243112,2.00525588832577,3.8));
#8773=CARTESIAN_POINT('',(-0.926794919243112,2.00525588832577,3.2));
#8774=CARTESIAN_POINT('',(-1.18660254037844,1.85525588832577,3.8));
#8775=CARTESIAN_POINT('',(-0.926794919243112,2.00525588832577,3.8));
#8776=CARTESIAN_POINT('',(-1.18660254037844,1.85525588832577,3.2));
#8777=CARTESIAN_POINT('Origin',(-3.69807621135331,0.405255888325767,3.2));
#8778=CARTESIAN_POINT('',(-3.39494366787712,3.28936938489376,3.2));
#8779=CARTESIAN_POINT('Origin',(-3.69807621135331,0.405255888325767,3.2));
#8780=CARTESIAN_POINT('',(-3.39494366787712,3.28936938489376,3.8));
#8781=CARTESIAN_POINT('Origin',(-3.69807621135331,0.405255888325767,3.8));
#8782=CARTESIAN_POINT('',(-3.39494366787712,3.28936938489376,3.2));
#8783=CARTESIAN_POINT('Origin',(-3.36358512889682,3.58772595350424,3.2));
#8784=CARTESIAN_POINT('',(-3.36358512889682,3.58772595350424,3.2));
#8785=CARTESIAN_POINT('',(-3.49891347099287,2.30016278581678,3.2));
#8786=CARTESIAN_POINT('',(-3.36358512889682,3.58772595350424,3.8));
#8787=CARTESIAN_POINT('',(-3.39494366787712,3.28936938489376,3.8));
#8788=CARTESIAN_POINT('',(-3.36358512889682,3.58772595350424,3.2));
#8789=CARTESIAN_POINT('Origin',(-3.69807621135332,0.405255888325766,3.2));
#8790=CARTESIAN_POINT('Origin',(-3.69807621135332,0.405255888325766,3.2));
#8791=CARTESIAN_POINT('Origin',(-3.69807621135332,0.405255888325766,3.8));
#8792=CARTESIAN_POINT('Origin',(-2.22154556813824,2.75240702699307,3.8));
#8793=CARTESIAN_POINT('Origin',(1.01339745962156,1.95525588832577,3.2));
#8794=CARTESIAN_POINT('',(1.27320508075689,1.80525588832577,3.2));
#8795=CARTESIAN_POINT('',(1.01339745962156,1.95525588832577,3.2));
#8796=CARTESIAN_POINT('',(3.30669872981078,0.631217782649107,3.2));
#8797=CARTESIAN_POINT('',(1.27320508075689,1.80525588832577,3.8));
#8798=CARTESIAN_POINT('',(1.27320508075689,1.80525588832577,3.2));
#8799=CARTESIAN_POINT('',(1.01339745962156,1.95525588832577,3.8));
#8800=CARTESIAN_POINT('',(1.27320508075689,1.80525588832577,3.8));
#8801=CARTESIAN_POINT('',(1.01339745962156,1.95525588832577,3.2));
#8802=CARTESIAN_POINT('Origin',(-1.49807621135331,3.40525588832576,3.2));
#8803=CARTESIAN_POINT('',(1.15120561581023,4.58479215324559,3.2));
#8804=CARTESIAN_POINT('Origin',(-1.49807621135331,3.40525588832576,3.2));
#8805=CARTESIAN_POINT('',(1.15120561581023,4.58479215324559,3.8));
#8806=CARTESIAN_POINT('Origin',(-1.49807621135331,3.40525588832576,3.8));
#8807=CARTESIAN_POINT('',(1.15120561581023,4.58479215324559,3.2));
#8808=CARTESIAN_POINT('Origin',(1.42526925310301,4.70681314616832,3.2));
#8809=CARTESIAN_POINT('',(1.42526925310301,4.70681314616833,3.2));
#8810=CARTESIAN_POINT('',(2.45976407096119,5.16739991388182,3.2));
#8811=CARTESIAN_POINT('',(1.42526925310301,4.70681314616833,3.8));
#8812=CARTESIAN_POINT('',(1.15120561581023,4.58479215324559,3.8));
#8813=CARTESIAN_POINT('',(1.42526925310301,4.70681314616833,3.2));
#8814=CARTESIAN_POINT('Origin',(-1.49807621135332,3.40525588832576,3.2));
#8815=CARTESIAN_POINT('Origin',(-1.49807621135332,3.40525588832576,3.2));
#8816=CARTESIAN_POINT('Origin',(-1.49807621135332,3.40525588832576,3.8));
#8817=CARTESIAN_POINT('Origin',(1.27288162286168,3.30011841116898,3.8));
#8818=CARTESIAN_POINT('Origin',(2.2,0.1,3.2));
#8819=CARTESIAN_POINT('',(2.2,-0.2,3.2));
#8820=CARTESIAN_POINT('',(2.2,0.1,3.2));
#8821=CARTESIAN_POINT('',(2.2,0.05,3.2));
#8822=CARTESIAN_POINT('',(2.2,-0.2,3.8));
#8823=CARTESIAN_POINT('',(2.2,-0.2,3.2));
#8824=CARTESIAN_POINT('',(2.2,0.1,3.8));
#8825=CARTESIAN_POINT('',(2.2,-0.2,3.8));
#8826=CARTESIAN_POINT('',(2.2,0.1,3.2));
#8827=CARTESIAN_POINT('Origin',(2.2,3.,3.2));
#8828=CARTESIAN_POINT('',(4.54614928368735,1.29542276835183,3.2));
#8829=CARTESIAN_POINT('Origin',(2.2,3.,3.2));
#8830=CARTESIAN_POINT('',(4.54614928368735,1.29542276835183,3.8));
#8831=CARTESIAN_POINT('Origin',(2.2,3.,3.8));
#8832=CARTESIAN_POINT('',(4.54614928368735,1.29542276835183,3.2));
#8833=CARTESIAN_POINT('Origin',(4.78885438199983,1.11908719266409,3.2));
#8834=CARTESIAN_POINT('',(4.78885438199983,1.11908719266409,3.2));
#8835=CARTESIAN_POINT('',(5.45128572287748,0.637802651632858,3.2));
#8836=CARTESIAN_POINT('',(4.78885438199983,1.11908719266409,3.8));
#8837=CARTESIAN_POINT('',(4.54614928368735,1.29542276835183,3.8));
#8838=CARTESIAN_POINT('',(4.78885438199983,1.11908719266409,3.2));
#8839=CARTESIAN_POINT('Origin',(2.2,3.,3.2));
#8840=CARTESIAN_POINT('Origin',(2.2,3.,3.2));
#8841=CARTESIAN_POINT('Origin',(2.2,3.,3.8));
#8842=CARTESIAN_POINT('Origin',(3.49442719099992,0.547711384175914,3.8));
#8843=CARTESIAN_POINT('Origin',(-2.85358983848623,-5.74256258422041,2.8));
#8844=CARTESIAN_POINT('',(-2.54668506678411,-5.21098792654702,3.2));
#8845=CARTESIAN_POINT('',(-2.54668506678411,-5.21098792654702,2.8));
#8846=CARTESIAN_POINT('',(-2.54668506678411,-5.21098792654702,2.8));
#8847=CARTESIAN_POINT('',(-2.74713149813783,-5.55817132984753,3.2));
#8848=CARTESIAN_POINT('',(-2.85358983848623,-5.74256258422041,3.2));
#8849=CARTESIAN_POINT('',(-2.74713149813783,-5.55817132984753,2.8));
#8850=CARTESIAN_POINT('',(-2.74713149813783,-5.55817132984753,0.));
#8851=CARTESIAN_POINT('',(-2.85358983848623,-5.74256258422041,2.8));
#8852=CARTESIAN_POINT('Origin',(-3.14641016151378,-4.64974226119285,2.8));
#8853=CARTESIAN_POINT('',(-3.23950538981167,-4.81098792654702,2.8));
#8854=CARTESIAN_POINT('',(-3.23950538981167,-4.81098792654702,3.2));
#8855=CARTESIAN_POINT('',(-3.23950538981167,-4.81098792654702,2.8));
#8856=CARTESIAN_POINT('',(-3.43995182116538,-5.15817132984752,2.8));
#8857=CARTESIAN_POINT('',(-3.14641016151378,-4.64974226119285,2.8));
#8858=CARTESIAN_POINT('',(-3.43995182116538,-5.15817132984752,3.2));
#8859=CARTESIAN_POINT('',(-3.43995182116538,-5.15817132984752,0.));
#8860=CARTESIAN_POINT('',(-3.14641016151378,-4.64974226119285,3.2));
#8861=CARTESIAN_POINT('Origin',(-3.54641016151377,5.34256258422041,2.8));
#8862=CARTESIAN_POINT('',(-3.23950538981166,4.81098792654702,3.2));
#8863=CARTESIAN_POINT('',(-3.23950538981166,4.81098792654702,2.8));
#8864=CARTESIAN_POINT('',(-3.23950538981166,4.81098792654702,2.8));
#8865=CARTESIAN_POINT('',(-3.43995182116538,5.15817132984753,3.2));
#8866=CARTESIAN_POINT('',(-3.54641016151377,5.34256258422041,3.2));
#8867=CARTESIAN_POINT('',(-3.43995182116538,5.15817132984753,2.8));
#8868=CARTESIAN_POINT('',(-3.43995182116538,5.15817132984753,0.));
#8869=CARTESIAN_POINT('',(-3.54641016151377,5.34256258422041,2.8));
#8870=CARTESIAN_POINT('Origin',(-2.45358983848622,5.04974226119286,2.8));
#8871=CARTESIAN_POINT('',(-2.54668506678411,5.21098792654702,2.8));
#8872=CARTESIAN_POINT('',(-2.54668506678411,5.21098792654702,3.2));
#8873=CARTESIAN_POINT('',(-2.54668506678411,5.21098792654702,2.8));
#8874=CARTESIAN_POINT('',(-2.74713149813783,5.55817132984753,2.8));
#8875=CARTESIAN_POINT('',(-2.45358983848622,5.04974226119286,2.8));
#8876=CARTESIAN_POINT('',(-2.74713149813783,5.55817132984753,3.2));
#8877=CARTESIAN_POINT('',(-2.74713149813783,5.55817132984753,0.));
#8878=CARTESIAN_POINT('',(-2.45358983848622,5.04974226119286,3.2));
#8879=CARTESIAN_POINT('Origin',(6.,0.,2.8));
#8880=CARTESIAN_POINT('Origin',(0.,0.,2.8));
#8881=CARTESIAN_POINT('Origin',(0.,0.,2.8));
#8882=CARTESIAN_POINT('',(5.78619045659577,0.4,2.8));
#8883=CARTESIAN_POINT('Origin',(0.,0.,2.8));
#8884=CARTESIAN_POINT('',(6.18708331930321,0.4,2.8));
#8885=CARTESIAN_POINT('',(6.4,0.4,2.8));
#8886=CARTESIAN_POINT('',(6.18708331930321,-0.4,2.8));
#8887=CARTESIAN_POINT('Origin',(0.,0.,2.8));
#8888=CARTESIAN_POINT('',(5.78619045659577,-0.4,2.8));
#8889=CARTESIAN_POINT('',(5.6,-0.4,2.8));
#8890=CARTESIAN_POINT('Origin',(0.,0.,2.8));
#8891=CARTESIAN_POINT('Origin',(0.,0.,2.8));
#8892=CARTESIAN_POINT('',(-1.7,-2.0818995585505E-16,2.8));
#8893=CARTESIAN_POINT('Origin',(0.,0.,2.8));
#8894=CARTESIAN_POINT('Origin',(0.,0.,2.8));
#8895=CARTESIAN_POINT('',(5.78619045659577,0.4,3.2));
#8896=CARTESIAN_POINT('Origin',(0.,0.,3.2));
#8897=CARTESIAN_POINT('',(5.78619045659577,0.4,2.8));
#8898=CARTESIAN_POINT('Origin',(0.,0.,2.8));
#8899=CARTESIAN_POINT('Origin',(0.,0.,3.2));
#8900=CARTESIAN_POINT('Origin',(0.,0.,2.8));
#8901=CARTESIAN_POINT('',(5.78619045659577,-0.4,3.2));
#8902=CARTESIAN_POINT('',(5.78619045659577,-0.4,2.8));
#8903=CARTESIAN_POINT('Origin',(0.,0.,3.2));
#8904=CARTESIAN_POINT('Origin',(0.,0.,2.8));
#8905=CARTESIAN_POINT('',(-1.7,-2.0818995585505E-16,3.2));
#8906=CARTESIAN_POINT('Origin',(0.,0.,3.2));
#8907=CARTESIAN_POINT('',(-1.7,-2.0818995585505E-16,2.8));
#8908=CARTESIAN_POINT('Origin',(6.,0.,3.2));
#8909=CARTESIAN_POINT('',(6.18708331930321,-0.4,3.2));
#8910=CARTESIAN_POINT('',(5.6,-0.4,3.2));
#8911=CARTESIAN_POINT('',(6.18708331930321,0.4,3.2));
#8912=CARTESIAN_POINT('Origin',(0.,0.,3.2));
#8913=CARTESIAN_POINT('',(6.4,0.4,3.2));
#8914=CARTESIAN_POINT('Origin',(0.,0.,3.2));
#8915=CARTESIAN_POINT('Origin',(0.,0.,3.2));
#8916=CARTESIAN_POINT('Origin',(5.6,-0.4,2.8));
#8917=CARTESIAN_POINT('',(6.18708331930321,-0.4,0.));
#8918=CARTESIAN_POINT('Origin',(6.4,0.4,2.8));
#8919=CARTESIAN_POINT('',(6.18708331930321,0.4,0.));
#8920=CARTESIAN_POINT('Origin',(0.,0.,0.));
#8921=CARTESIAN_POINT('',(-6.2,-7.59281015471359E-16,0.));
#8922=CARTESIAN_POINT('',(-6.2,-7.59281015471359E-16,0.));
#8923=CARTESIAN_POINT('Origin',(0.,0.,0.));
#8924=CARTESIAN_POINT('Origin',(0.,0.,0.));
#8925=CARTESIAN_POINT('',(-8.2,-1.00421037530083E-15,3.8));
#8926=CARTESIAN_POINT('Origin',(0.,0.,3.8));
#8927=CARTESIAN_POINT('',(-8.2,-1.00421037530083E-15,0.));
#8928=CARTESIAN_POINT('',(-8.2,-1.00421037530083E-15,0.));
#8929=CARTESIAN_POINT('Origin',(0.,0.,0.));
#8930=CARTESIAN_POINT('Origin',(0.,0.,3.8));
#8931=CARTESIAN_POINT('Origin',(0.,0.,0.));
#8932=CARTESIAN_POINT('',(0.,0.,0.));
#8933=CARTESIAN_POINT('Origin',(0.,0.,4.2));
#8934=CARTESIAN_POINT('',(-6.35,-7.77650717458569E-16,4.2));
#8935=CARTESIAN_POINT('Origin',(0.,0.,4.2));
#8936=CARTESIAN_POINT('',(-6.35,-7.77650717458569E-16,4.));
#8937=CARTESIAN_POINT('',(-6.35,7.77650717458569E-16,4.2));
#8938=CARTESIAN_POINT('Origin',(0.,0.,4.));
#8939=CARTESIAN_POINT('Origin',(0.,0.,4.2));
#8940=CARTESIAN_POINT('',(-6.85,-8.38883057415937E-16,4.2));
#8941=CARTESIAN_POINT('Origin',(0.,0.,4.2));
#8942=CARTESIAN_POINT('',(-6.85,-8.38883057415937E-16,4.));
#8943=CARTESIAN_POINT('',(-6.85,8.38883057415937E-16,4.2));
#8944=CARTESIAN_POINT('Origin',(0.,0.,4.));
#8945=CARTESIAN_POINT('Origin',(0.,0.,4.));
#8946=CARTESIAN_POINT('Origin',(0.,0.,4.2));
#8947=CARTESIAN_POINT('',(-2.7,-3.30654635769785E-16,4.2));
#8948=CARTESIAN_POINT('Origin',(0.,0.,4.2));
#8949=CARTESIAN_POINT('Origin',(-7.4,0.,4.));
#8950=CARTESIAN_POINT('',(-7.75,4.28626379701574E-17,4.2));
#8951=CARTESIAN_POINT('Origin',(-7.4,0.,4.2));
#8952=CARTESIAN_POINT('',(-7.75,4.28626379701574E-17,3.8));
#8953=CARTESIAN_POINT('',(-7.75,4.28626379701574E-17,4.));
#8954=CARTESIAN_POINT('Origin',(-7.4,0.,3.8));
#8955=CARTESIAN_POINT('Origin',(7.4,0.,4.));
#8956=CARTESIAN_POINT('',(7.05,4.28626379701574E-17,4.2));
#8957=CARTESIAN_POINT('Origin',(7.4,0.,4.2));
#8958=CARTESIAN_POINT('',(7.05,4.28626379701574E-17,3.8));
#8959=CARTESIAN_POINT('',(7.05,4.28626379701574E-17,4.));
#8960=CARTESIAN_POINT('Origin',(7.4,0.,3.8));
#8961=CARTESIAN_POINT('Origin',(0.,7.4,4.));
#8962=CARTESIAN_POINT('',(-0.35,7.4,4.2));
#8963=CARTESIAN_POINT('Origin',(0.,7.4,4.2));
#8964=CARTESIAN_POINT('',(-0.35,7.4,3.8));
#8965=CARTESIAN_POINT('',(-0.35,7.4,4.));
#8966=CARTESIAN_POINT('Origin',(0.,7.4,3.8));
#8967=CARTESIAN_POINT('Origin',(0.,-7.4,4.));
#8968=CARTESIAN_POINT('',(-0.35,-7.4,4.2));
#8969=CARTESIAN_POINT('Origin',(0.,-7.4,4.2));
#8970=CARTESIAN_POINT('',(-0.35,-7.4,3.8));
#8971=CARTESIAN_POINT('',(-0.35,-7.4,4.));
#8972=CARTESIAN_POINT('Origin',(0.,-7.4,3.8));
#8973=CARTESIAN_POINT('Origin',(0.,0.,3.8));
#8974=CARTESIAN_POINT('',(-2.7,-3.30654635769785E-16,3.8));
#8975=CARTESIAN_POINT('',(-2.7,-3.30654635769785E-16,3.8));
#8976=CARTESIAN_POINT('Origin',(0.,0.,3.8));
#8977=CARTESIAN_POINT('Origin',(0.,0.,3.8));
#8978=CARTESIAN_POINT('',(-8.2,-1.00421037530083E-15,4.2));
#8979=CARTESIAN_POINT('Origin',(0.,0.,4.2));
#8980=CARTESIAN_POINT('',(-8.2,-1.00421037530083E-15,3.8));
#8981=CARTESIAN_POINT('',(-8.2,-1.00421037530083E-15,3.8));
#8982=CARTESIAN_POINT('Origin',(0.,0.,3.8));
#8983=CARTESIAN_POINT('Origin',(0.,0.,4.2));
#8984=CARTESIAN_POINT('Origin',(0.,0.,3.8));
#8985=CARTESIAN_POINT('',(0.,0.,0.));
#8986=CARTESIAN_POINT('Origin',(1.3,-0.3,3.));
#8987=CARTESIAN_POINT('',(0.953939201416946,-0.3,3.));
#8988=CARTESIAN_POINT('',(0.953939201416946,-0.3,1.8));
#8989=CARTESIAN_POINT('',(0.953939201416946,-0.3,1.8));
#8990=CARTESIAN_POINT('',(1.3,-0.3,3.));
#8991=CARTESIAN_POINT('',(0.7,-0.3,3.));
#8992=CARTESIAN_POINT('',(1.3,-0.3,1.8));
#8993=CARTESIAN_POINT('',(1.3,-0.3,3.));
#8994=CARTESIAN_POINT('',(0.65,-0.3,1.8));
#8995=CARTESIAN_POINT('Origin',(1.3,0.3,3.));
#8996=CARTESIAN_POINT('',(1.3,0.3,3.));
#8997=CARTESIAN_POINT('',(1.3,-0.3,3.));
#8998=CARTESIAN_POINT('',(1.3,0.3,1.8));
#8999=CARTESIAN_POINT('',(1.3,0.3,3.));
#9000=CARTESIAN_POINT('',(1.3,0.15,1.8));
#9001=CARTESIAN_POINT('Origin',(0.7,0.3,3.));
#9002=CARTESIAN_POINT('',(0.953939201416946,0.3,1.8));
#9003=CARTESIAN_POINT('',(0.953939201416946,0.3,3.));
#9004=CARTESIAN_POINT('',(0.953939201416946,0.3,1.8));
#9005=CARTESIAN_POINT('',(0.35,0.3,1.8));
#9006=CARTESIAN_POINT('',(1.3,0.3,3.));
#9007=CARTESIAN_POINT('Origin',(1.,0.,3.));
#9008=CARTESIAN_POINT('Origin',(0.,0.,3.));
#9009=CARTESIAN_POINT('Origin',(0.,0.,1.8));
#9010=CARTESIAN_POINT('',(-5.,-6.12323399573677E-16,1.8));
#9011=CARTESIAN_POINT('Origin',(0.,0.,1.8));
#9012=CARTESIAN_POINT('',(1.01339745962155,-1.95525588832577,1.8));
#9013=CARTESIAN_POINT('',(1.15120561581022,-4.58479215324559,1.8));
#9014=CARTESIAN_POINT('Origin',(-1.49807621135332,-3.40525588832576,1.8));
#9015=CARTESIAN_POINT('',(1.425269253103,-4.70681314616833,1.8));
#9016=CARTESIAN_POINT('',(-0.180963657223493,-3.99167217920436,1.8));
#9017=CARTESIAN_POINT('',(1.27320508075689,-1.80525588832577,1.8));
#9018=CARTESIAN_POINT('Origin',(-1.49807621135332,-3.40525588832576,1.8));
#9019=CARTESIAN_POINT('',(1.18660254037844,-1.85525588832577,1.8));
#9020=CARTESIAN_POINT('',(-1.18660254037845,-1.85525588832576,1.8));
#9021=CARTESIAN_POINT('',(-3.39494366787712,-3.28936938489376,1.8));
#9022=CARTESIAN_POINT('Origin',(-3.69807621135331,-0.405255888325764,1.8));
#9023=CARTESIAN_POINT('',(-3.36358512889683,-3.58772595350424,1.8));
#9024=CARTESIAN_POINT('',(-3.54737133938231,-1.8391169652849,1.8));
#9025=CARTESIAN_POINT('',(-0.926794919243113,-2.00525588832576,1.8));
#9026=CARTESIAN_POINT('Origin',(-3.69807621135332,-0.405255888325764,1.8));
#9027=CARTESIAN_POINT('',(-1.01339745962156,-1.95525588832576,1.8));
#9028=CARTESIAN_POINT('',(-2.2,0.1,1.8));
#9029=CARTESIAN_POINT('',(-4.54614928368735,1.29542276835183,1.8));
#9030=CARTESIAN_POINT('Origin',(-2.2,3.,1.8));
#9031=CARTESIAN_POINT('',(-4.78885438199983,1.11908719266409,1.8));
#9032=CARTESIAN_POINT('',(-3.36640768215882,2.15255521391946,1.8));
#9033=CARTESIAN_POINT('',(-2.2,-0.2,1.8));
#9034=CARTESIAN_POINT('Origin',(-2.2,3.,1.8));
#9035=CARTESIAN_POINT('',(-2.2,-0.0999999999999997,1.8));
#9036=CARTESIAN_POINT('',(-1.01339745962156,1.95525588832577,1.8));
#9037=CARTESIAN_POINT('',(-1.15120561581023,4.58479215324559,1.8));
#9038=CARTESIAN_POINT('Origin',(1.49807621135331,3.40525588832576,1.8));
#9039=CARTESIAN_POINT('',(-1.42526925310301,4.70681314616833,1.8));
#9040=CARTESIAN_POINT('',(0.18096365722349,3.99167217920436,1.8));
#9041=CARTESIAN_POINT('',(-1.27320508075689,1.80525588832577,1.8));
#9042=CARTESIAN_POINT('Origin',(1.49807621135332,3.40525588832576,1.8));
#9043=CARTESIAN_POINT('',(-1.18660254037844,1.85525588832577,1.8));
#9044=CARTESIAN_POINT('',(1.18660254037844,1.85525588832577,1.8));
#9045=CARTESIAN_POINT('',(3.39494366787712,3.28936938489376,1.8));
#9046=CARTESIAN_POINT('Origin',(3.69807621135331,0.405255888325766,1.8));
#9047=CARTESIAN_POINT('',(3.36358512889683,3.58772595350424,1.8));
#9048=CARTESIAN_POINT('',(3.54737133938231,1.8391169652849,1.8));
#9049=CARTESIAN_POINT('',(0.926794919243113,2.00525588832576,1.8));
#9050=CARTESIAN_POINT('Origin',(3.69807621135332,0.405255888325765,1.8));
#9051=CARTESIAN_POINT('',(1.01339745962156,1.95525588832577,1.8));
#9052=CARTESIAN_POINT('',(2.2,-0.1,1.8));
#9053=CARTESIAN_POINT('',(4.54614928368735,-1.29542276835183,1.8));
#9054=CARTESIAN_POINT('Origin',(2.2,-3.,1.8));
#9055=CARTESIAN_POINT('',(4.78885438199983,-1.11908719266409,1.8));
#9056=CARTESIAN_POINT('',(3.36640768215882,-2.15255521391946,1.8));
#9057=CARTESIAN_POINT('',(2.2,0.2,1.8));
#9058=CARTESIAN_POINT('Origin',(2.2,-3.,1.8));
#9059=CARTESIAN_POINT('',(2.2,0.1,1.8));
#9060=CARTESIAN_POINT('',(-1.,-1.22464679914735E-16,1.8));
#9061=CARTESIAN_POINT('Origin',(0.,0.,1.8));
#9062=CARTESIAN_POINT('Origin',(0.,0.,1.8));
#9063=CARTESIAN_POINT('Origin',(-1.49807621135332,-3.40525588832576,0.8));
#9064=CARTESIAN_POINT('',(1.15120561581022,-4.58479215324559,0.8));
#9065=CARTESIAN_POINT('',(1.01339745962155,-1.95525588832577,0.8));
#9066=CARTESIAN_POINT('Origin',(-1.49807621135332,-3.40525588832576,0.8));
#9067=CARTESIAN_POINT('',(1.15120561581022,-4.58479215324559,0.8));
#9068=CARTESIAN_POINT('',(1.01339745962155,-1.95525588832577,0.8));
#9069=CARTESIAN_POINT('Origin',(1.27320508075689,-1.80525588832577,0.8));
#9070=CARTESIAN_POINT('',(1.27320508075689,-1.80525588832577,0.8));
#9071=CARTESIAN_POINT('',(1.27320508075689,-1.80525588832577,0.8));
#9072=CARTESIAN_POINT('',(1.27320508075689,-1.80525588832577,0.8));
#9073=CARTESIAN_POINT('Origin',(-1.49807621135332,-3.40525588832576,0.8));
#9074=CARTESIAN_POINT('',(1.425269253103,-4.70681314616833,0.8));
#9075=CARTESIAN_POINT('Origin',(-1.49807621135332,-3.40525588832576,0.8));
#9076=CARTESIAN_POINT('',(1.425269253103,-4.70681314616833,0.8));
#9077=CARTESIAN_POINT('Origin',(1.15120561581022,-4.58479215324559,0.8));
#9078=CARTESIAN_POINT('',(1.15120561581022,-4.58479215324559,0.8));
#9079=CARTESIAN_POINT('Origin',(1.27288162286168,-3.30011841116898,0.8));
#9080=CARTESIAN_POINT('Origin',(-3.69807621135331,-0.405255888325764,0.8));
#9081=CARTESIAN_POINT('',(-3.39494366787712,-3.28936938489376,0.8));
#9082=CARTESIAN_POINT('',(-1.18660254037845,-1.85525588832576,0.8));
#9083=CARTESIAN_POINT('Origin',(-3.69807621135331,-0.405255888325764,0.8));
#9084=CARTESIAN_POINT('',(-3.39494366787712,-3.28936938489376,0.8));
#9085=CARTESIAN_POINT('',(-1.18660254037845,-1.85525588832576,0.8));
#9086=CARTESIAN_POINT('Origin',(-0.926794919243113,-2.00525588832576,0.8));
#9087=CARTESIAN_POINT('',(-0.926794919243113,-2.00525588832576,0.8));
#9088=CARTESIAN_POINT('',(-0.926794919243113,-2.00525588832576,0.8));
#9089=CARTESIAN_POINT('',(-0.926794919243113,-2.00525588832576,0.8));
#9090=CARTESIAN_POINT('Origin',(-3.69807621135332,-0.405255888325764,0.8));
#9091=CARTESIAN_POINT('',(-3.36358512889683,-3.58772595350424,0.8));
#9092=CARTESIAN_POINT('Origin',(-3.69807621135332,-0.405255888325764,0.8));
#9093=CARTESIAN_POINT('',(-3.36358512889683,-3.58772595350424,0.8));
#9094=CARTESIAN_POINT('Origin',(-3.39494366787712,-3.28936938489376,0.8));
#9095=CARTESIAN_POINT('',(-3.39494366787712,-3.28936938489376,0.8));
#9096=CARTESIAN_POINT('Origin',(-2.22154556813824,-2.75240702699307,0.8));
#9097=CARTESIAN_POINT('Origin',(-2.2,3.,0.8));
#9098=CARTESIAN_POINT('',(-4.54614928368735,1.29542276835183,0.8));
#9099=CARTESIAN_POINT('',(-2.2,0.1,0.8));
#9100=CARTESIAN_POINT('Origin',(-2.2,3.,0.8));
#9101=CARTESIAN_POINT('',(-4.54614928368735,1.29542276835183,0.8));
#9102=CARTESIAN_POINT('',(-2.2,0.1,0.8));
#9103=CARTESIAN_POINT('Origin',(-2.2,-0.2,0.8));
#9104=CARTESIAN_POINT('',(-2.2,-0.2,0.8));
#9105=CARTESIAN_POINT('',(-2.2,-0.2,0.8));
#9106=CARTESIAN_POINT('',(-2.2,-0.2,0.8));
#9107=CARTESIAN_POINT('Origin',(-2.2,3.,0.8));
#9108=CARTESIAN_POINT('',(-4.78885438199983,1.11908719266409,0.8));
#9109=CARTESIAN_POINT('Origin',(-2.2,3.,0.8));
#9110=CARTESIAN_POINT('',(-4.78885438199983,1.11908719266409,0.8));
#9111=CARTESIAN_POINT('Origin',(-4.54614928368735,1.29542276835183,0.8));
#9112=CARTESIAN_POINT('',(-4.54614928368735,1.29542276835183,0.8));
#9113=CARTESIAN_POINT('Origin',(-3.49442719099992,0.547711384175914,0.8));
#9114=CARTESIAN_POINT('Origin',(1.49807621135331,3.40525588832576,0.8));
#9115=CARTESIAN_POINT('',(-1.15120561581023,4.58479215324559,0.8));
#9116=CARTESIAN_POINT('',(-1.01339745962156,1.95525588832577,0.8));
#9117=CARTESIAN_POINT('Origin',(1.49807621135331,3.40525588832576,0.8));
#9118=CARTESIAN_POINT('',(-1.15120561581023,4.58479215324559,0.8));
#9119=CARTESIAN_POINT('',(-1.01339745962156,1.95525588832577,0.8));
#9120=CARTESIAN_POINT('Origin',(-1.27320508075689,1.80525588832577,0.8));
#9121=CARTESIAN_POINT('',(-1.27320508075689,1.80525588832577,0.8));
#9122=CARTESIAN_POINT('',(-1.27320508075689,1.80525588832577,0.8));
#9123=CARTESIAN_POINT('',(-1.27320508075689,1.80525588832577,0.8));
#9124=CARTESIAN_POINT('Origin',(1.49807621135332,3.40525588832576,0.8));
#9125=CARTESIAN_POINT('',(-1.42526925310301,4.70681314616833,0.8));
#9126=CARTESIAN_POINT('Origin',(1.49807621135332,3.40525588832576,0.8));
#9127=CARTESIAN_POINT('',(-1.42526925310301,4.70681314616833,0.8));
#9128=CARTESIAN_POINT('Origin',(-1.15120561581023,4.58479215324559,0.8));
#9129=CARTESIAN_POINT('',(-1.15120561581023,4.58479215324559,0.8));
#9130=CARTESIAN_POINT('Origin',(-1.27288162286168,3.30011841116898,0.8));
#9131=CARTESIAN_POINT('Origin',(3.69807621135331,0.405255888325766,0.8));
#9132=CARTESIAN_POINT('',(3.39494366787712,3.28936938489376,0.8));
#9133=CARTESIAN_POINT('',(1.18660254037844,1.85525588832577,0.8));
#9134=CARTESIAN_POINT('Origin',(3.69807621135331,0.405255888325766,0.8));
#9135=CARTESIAN_POINT('',(3.39494366787712,3.28936938489376,0.8));
#9136=CARTESIAN_POINT('',(1.18660254037844,1.85525588832577,0.8));
#9137=CARTESIAN_POINT('Origin',(0.926794919243113,2.00525588832576,0.8));
#9138=CARTESIAN_POINT('',(0.926794919243113,2.00525588832576,0.8));
#9139=CARTESIAN_POINT('',(0.926794919243113,2.00525588832576,0.8));
#9140=CARTESIAN_POINT('',(0.926794919243113,2.00525588832576,0.8));
#9141=CARTESIAN_POINT('Origin',(3.69807621135332,0.405255888325765,0.8));
#9142=CARTESIAN_POINT('',(3.36358512889683,3.58772595350424,0.8));
#9143=CARTESIAN_POINT('Origin',(3.69807621135332,0.405255888325765,0.8));
#9144=CARTESIAN_POINT('',(3.36358512889683,3.58772595350424,0.8));
#9145=CARTESIAN_POINT('Origin',(3.39494366787712,3.28936938489376,0.8));
#9146=CARTESIAN_POINT('',(3.39494366787712,3.28936938489376,0.8));
#9147=CARTESIAN_POINT('Origin',(2.22154556813824,2.75240702699307,0.8));
#9148=CARTESIAN_POINT('Origin',(2.2,-3.,0.8));
#9149=CARTESIAN_POINT('',(4.54614928368735,-1.29542276835183,0.8));
#9150=CARTESIAN_POINT('',(2.2,-0.1,0.8));
#9151=CARTESIAN_POINT('Origin',(2.2,-3.,0.8));
#9152=CARTESIAN_POINT('',(4.54614928368735,-1.29542276835183,0.8));
#9153=CARTESIAN_POINT('',(2.2,-0.1,0.8));
#9154=CARTESIAN_POINT('Origin',(2.2,0.2,0.8));
#9155=CARTESIAN_POINT('',(2.2,0.2,0.8));
#9156=CARTESIAN_POINT('',(2.2,0.2,0.8));
#9157=CARTESIAN_POINT('',(2.2,0.2,0.8));
#9158=CARTESIAN_POINT('Origin',(2.2,-3.,0.8));
#9159=CARTESIAN_POINT('',(4.78885438199983,-1.11908719266409,0.8));
#9160=CARTESIAN_POINT('Origin',(2.2,-3.,0.8));
#9161=CARTESIAN_POINT('',(4.78885438199983,-1.11908719266409,0.8));
#9162=CARTESIAN_POINT('Origin',(4.54614928368735,-1.29542276835183,0.8));
#9163=CARTESIAN_POINT('',(4.54614928368735,-1.29542276835183,0.8));
#9164=CARTESIAN_POINT('Origin',(3.49442719099992,-0.547711384175914,0.8));
#9165=CARTESIAN_POINT('Origin',(0.,0.,2.2));
#9166=CARTESIAN_POINT('',(-1.5,-1.83697019872103E-16,3.2));
#9167=CARTESIAN_POINT('Origin',(0.,0.,3.2));
#9168=CARTESIAN_POINT('',(-1.5,-1.83697019872103E-16,2.2));
#9169=CARTESIAN_POINT('',(-1.5,-1.83697019872103E-16,2.2));
#9170=CARTESIAN_POINT('Origin',(0.,0.,2.2));
#9171=CARTESIAN_POINT('Origin',(0.,0.,3.2));
#9172=CARTESIAN_POINT('',(-1.,-1.22464679914735E-16,3.2));
#9173=CARTESIAN_POINT('Origin',(0.,0.,3.2));
#9174=CARTESIAN_POINT('Origin',(0.,0.,1.8));
#9175=CARTESIAN_POINT('',(-1.,-1.22464679914735E-16,1.8));
#9176=CARTESIAN_POINT('Origin',(0.,0.,1.8));
#9177=CARTESIAN_POINT('',(-5.,-6.12323399573677E-16,2.2));
#9178=CARTESIAN_POINT('Origin',(0.,0.,2.2));
#9179=CARTESIAN_POINT('',(-5.,-6.12323399573677E-16,1.8));
#9180=CARTESIAN_POINT('Origin',(0.,0.,2.2));
#9181=CARTESIAN_POINT('',(0.,0.,0.));
#9182=CARTESIAN_POINT('Origin',(0.,0.,0.));
#9183=CARTESIAN_POINT('',(-1.5,-1.83697019872103E-16,0.4));
#9184=CARTESIAN_POINT('Origin',(0.,0.,0.4));
#9185=CARTESIAN_POINT('',(-1.5,-1.83697019872103E-16,0.));
#9186=CARTESIAN_POINT('',(-1.5,-1.83697019872103E-16,0.));
#9187=CARTESIAN_POINT('Origin',(0.,0.,0.));
#9188=CARTESIAN_POINT('Origin',(0.,0.,0.));
#9189=CARTESIAN_POINT('',(-1.7,-2.0818995585505E-16,0.4));
#9190=CARTESIAN_POINT('Origin',(0.,0.,0.4));
#9191=CARTESIAN_POINT('',(-1.7,-2.0818995585505E-16,0.));
#9192=CARTESIAN_POINT('',(-1.7,-2.0818995585505E-16,0.));
#9193=CARTESIAN_POINT('Origin',(0.,0.,0.));
#9194=CARTESIAN_POINT('Origin',(0.,0.,0.4));
#9195=CARTESIAN_POINT('Origin',(0.,0.,0.));
#9196=CARTESIAN_POINT('',(0.,0.,0.));
#9197=CARTESIAN_POINT('Origin',(0.,-7.4,-0.45));
#9198=CARTESIAN_POINT('',(-0.251358478231671,-7.40000989059476,-0.761258330249198));
#9199=CARTESIAN_POINT('',(-0.251584539328545,-7.40033372506469,-0.788741669750802));
#9200=CARTESIAN_POINT('',(-0.25175,-7.4,-0.45));
#9201=CARTESIAN_POINT('',(-0.191346599666506,-7.23640127966251,-0.8));
#9202=CARTESIAN_POINT('Ctrl Pts',(-0.251584539328545,-7.40033372506469,
-0.788741669750802));
#9203=CARTESIAN_POINT('Ctrl Pts',(-0.251071222245464,-7.34107836270979,
-0.792494446500535));
#9204=CARTESIAN_POINT('Ctrl Pts',(-0.229922182808405,-7.28151964396956,
-0.796247223250268));
#9205=CARTESIAN_POINT('Ctrl Pts',(-0.191346599666506,-7.23640127966251,
-0.8));
#9206=CARTESIAN_POINT('',(0.191702374352699,-7.23617294219443,-0.8));
#9207=CARTESIAN_POINT('Origin',(0.,-7.4,-0.8));
#9208=CARTESIAN_POINT('Ctrl Pts',(0.191704041017362,-7.23617187252308,-0.8));
#9209=CARTESIAN_POINT('Ctrl Pts',(0.140332563765971,-7.17646166153928,-0.795000212253756));
#9210=CARTESIAN_POINT('Ctrl Pts',(0.0585928763053871,-7.14242248557627,
-0.790000424507512));
#9211=CARTESIAN_POINT('Ctrl Pts',(-0.0199179743947309,-7.14865374913574,
-0.785000636761267));
#9212=CARTESIAN_POINT('Ctrl Pts',(-0.102096219979331,-7.15517608716323,
-0.779767299182859));
#9213=CARTESIAN_POINT('Ctrl Pts',(-0.180736932942895,-7.20581895652833,
-0.77453396160445));
#9214=CARTESIAN_POINT('Ctrl Pts',(-0.220629120750179,-7.27793230721061,
-0.769300624026042));
#9215=CARTESIAN_POINT('Ctrl Pts',(-0.241063798043618,-7.314872197719,-0.766619859433761));
#9216=CARTESIAN_POINT('Ctrl Pts',(-0.251330955357681,-7.35744589098191,
-0.763939094841479));
#9217=CARTESIAN_POINT('Ctrl Pts',(-0.251358478231671,-7.40000989059476,
-0.761258330249198));
#9218=CARTESIAN_POINT('Origin',(0.,-7.4,-0.45));
#9219=CARTESIAN_POINT('',(-0.252017165498346,-7.40015401716005,-0.661258330249198));
#9220=CARTESIAN_POINT('',(-0.252073448596348,-7.39987961136196,-0.688741669750803));
#9221=CARTESIAN_POINT('',(-0.25175,-7.4,-0.45));
#9222=CARTESIAN_POINT('Ctrl Pts',(-0.252073448596348,-7.39987961136196,
-0.688741669750803));
#9223=CARTESIAN_POINT('Ctrl Pts',(-0.25211567655556,-7.3927435289656,-0.689194416785009));
#9224=CARTESIAN_POINT('Ctrl Pts',(-0.251838292098126,-7.38561079836488,
-0.689647163819216));
#9225=CARTESIAN_POINT('Ctrl Pts',(-0.251230519881648,-7.37850635975571,
-0.690099910853423));
#9226=CARTESIAN_POINT('Ctrl Pts',(-0.244205234370541,-7.29638561077722,
-0.695333248431831));
#9227=CARTESIAN_POINT('Ctrl Pts',(-0.193036097579369,-7.21804501839796,
-0.700566586010239));
#9228=CARTESIAN_POINT('Ctrl Pts',(-0.12066406959885,-7.17860007027604,-0.705799923588648));
#9229=CARTESIAN_POINT('Ctrl Pts',(-0.0482920416183288,-7.13915512215413,
-0.711033261167056));
#9230=CARTESIAN_POINT('Ctrl Pts',(0.0452828775515399,-7.13860581828957,
-0.716266598745465));
#9231=CARTESIAN_POINT('Ctrl Pts',(0.118103971990326,-7.17721638163908,-0.721499936323874));
#9232=CARTESIAN_POINT('Ctrl Pts',(0.190925066429111,-7.21582694498859,-0.726733273902282));
#9233=CARTESIAN_POINT('Ctrl Pts',(0.242992336136814,-7.29359737555218,-0.73196661148069));
#9234=CARTESIAN_POINT('Ctrl Pts',(0.250965104406924,-7.37562272577954,-0.737199949059099));
#9235=CARTESIAN_POINT('Ctrl Pts',(0.258937872677034,-7.4576480760069,-0.742433286637507));
#9236=CARTESIAN_POINT('Ctrl Pts',(0.22281613950955,-7.54392834589802,-0.747666624215916));
#9237=CARTESIAN_POINT('Ctrl Pts',(0.158787402101112,-7.59585258416295,-0.752899961794324));
#9238=CARTESIAN_POINT('Ctrl Pts',(0.0947586646926728,-7.64777682242788,
-0.758133299372733));
#9239=CARTESIAN_POINT('Ctrl Pts',(0.0028229230432783,-7.66534502906661,
-0.763366636951141));
#9240=CARTESIAN_POINT('Ctrl Pts',(-0.0757847496475859,-7.64053050273058,
-0.76859997452955));
#9241=CARTESIAN_POINT('Ctrl Pts',(-0.154392422338449,-7.61571597639454,
-0.773833312107958));
#9242=CARTESIAN_POINT('Ctrl Pts',(-0.219672026070782,-7.54851871708374,
-0.779066649686366));
#9243=CARTESIAN_POINT('Ctrl Pts',(-0.242359215388134,-7.46941970437215,
-0.784299987264775));
#9244=CARTESIAN_POINT('Ctrl Pts',(-0.248777636388646,-7.44704184358004,
-0.78578054809345));
#9245=CARTESIAN_POINT('Ctrl Pts',(-0.251787055283152,-7.42371139292034,
-0.787261108922126));
#9246=CARTESIAN_POINT('Ctrl Pts',(-0.251584539328545,-7.40033372506469,
-0.788741669750802));
#9247=CARTESIAN_POINT('Ctrl Pts',(-0.251358478231671,-7.40000989059476,
-0.761258330249198));
#9248=CARTESIAN_POINT('Ctrl Pts',(-0.251384684988075,-7.44053852033946,
-0.758705757263071));
#9249=CARTESIAN_POINT('Ctrl Pts',(-0.242127141836486,-7.4810583613502,-0.756153184276944));
#9250=CARTESIAN_POINT('Ctrl Pts',(-0.223523592831821,-7.51669741987088,
-0.753600611290817));
#9251=CARTESIAN_POINT('Ctrl Pts',(-0.185382214455175,-7.58976534984939,
-0.748367273712408));
#9252=CARTESIAN_POINT('Ctrl Pts',(-0.107955795050881,-7.64231737780695,
-0.743133936134));
#9253=CARTESIAN_POINT('Ctrl Pts',(-0.0259706133934279,-7.65080523818006,
-0.737900598555591));
#9254=CARTESIAN_POINT('Ctrl Pts',(0.0560145682640249,-7.65929309855318,
-0.732667260977183));
#9255=CARTESIAN_POINT('Ctrl Pts',(0.142558512174636,-7.62371679134186,-0.727433923398774));
#9256=CARTESIAN_POINT('Ctrl Pts',(0.194864662021149,-7.56002033893795,-0.722200585820366));
#9257=CARTESIAN_POINT('Ctrl Pts',(0.247170811867661,-7.49632388653404,-0.716967248241958));
#9258=CARTESIAN_POINT('Ctrl Pts',(0.265239167650075,-7.40450728893754,-0.71173391066355));
#9259=CARTESIAN_POINT('Ctrl Pts',(0.240965802115707,-7.32574032208645,-0.706500573085141));
#9260=CARTESIAN_POINT('Ctrl Pts',(0.216692436581339,-7.24697335523537,-0.701267235506732));
#9261=CARTESIAN_POINT('Ctrl Pts',(0.150077349730189,-7.1812560191297,-0.696033897928324));
#9262=CARTESIAN_POINT('Ctrl Pts',(0.0709891696492391,-7.15805132892677,
-0.690800560349915));
#9263=CARTESIAN_POINT('Ctrl Pts',(-0.00809901043171256,-7.13484663872384,
-0.685567222771507));
#9264=CARTESIAN_POINT('Ctrl Pts',(-0.0996602837424652,-7.15415459442365,
-0.680333885193099));
#9265=CARTESIAN_POINT('Ctrl Pts',(-0.162643425289155,-7.20731920825571,
-0.675100547614691));
#9266=CARTESIAN_POINT('Ctrl Pts',(-0.218173720095525,-7.2541928097761,-0.670486475159527));
#9267=CARTESIAN_POINT('Ctrl Pts',(-0.251489074403517,-7.32738456435463,
-0.665872402704362));
#9268=CARTESIAN_POINT('Ctrl Pts',(-0.252017165498346,-7.40015401716005,
-0.661258330249198));
#9269=CARTESIAN_POINT('Origin',(0.,-7.4,-0.45));
#9270=CARTESIAN_POINT('',(-0.251711685022834,-7.3997833335225,-0.561258330249198));
#9271=CARTESIAN_POINT('',(-0.25137527833601,-7.39994331833701,-0.588741669750803));
#9272=CARTESIAN_POINT('',(-0.25175,-7.4,-0.45));
#9273=CARTESIAN_POINT('Ctrl Pts',(-0.25137527833601,-7.39994331833701,-0.588741669750803));
#9274=CARTESIAN_POINT('Ctrl Pts',(-0.251453232926026,-7.36206606061581,
-0.591127724647892));
#9275=CARTESIAN_POINT('Ctrl Pts',(-0.243409884741493,-7.32422023730893,
-0.593513779544982));
#9276=CARTESIAN_POINT('Ctrl Pts',(-0.227072436774608,-7.29037848576413,
-0.595899834442071));
#9277=CARTESIAN_POINT('Ctrl Pts',(-0.191239489056313,-7.21615332426654,
-0.601133172020479));
#9278=CARTESIAN_POINT('Ctrl Pts',(-0.115507184704655,-7.16119003463128,
-0.606366509598888));
#9279=CARTESIAN_POINT('Ctrl Pts',(-0.0338304512848064,-7.15013153945356,
-0.611599847177296));
#9280=CARTESIAN_POINT('Ctrl Pts',(0.0478462821350425,-7.13907304427583,
-0.616833184755704));
#9281=CARTESIAN_POINT('Ctrl Pts',(0.135467444623083,-7.17191934355563,-0.622066522334113));
#9282=CARTESIAN_POINT('Ctrl Pts',(0.189747638705398,-7.23394390765325,-0.627299859912521));
#9283=CARTESIAN_POINT('Ctrl Pts',(0.244027832787713,-7.29596847175088,-0.63253319749093));
#9284=CARTESIAN_POINT('Ctrl Pts',(0.264967058464304,-7.38717130066634,-0.637766535069338));
#9285=CARTESIAN_POINT('Ctrl Pts',(0.243177171908073,-7.46666063157891,-0.642999872647747));
#9286=CARTESIAN_POINT('Ctrl Pts',(0.221387285351841,-7.54614996249148,-0.648233210226155));
#9287=CARTESIAN_POINT('Ctrl Pts',(0.156868286562786,-7.61392579540117,-0.653466547804563));
#9288=CARTESIAN_POINT('Ctrl Pts',(0.0785474602301629,-7.63960159378581,
-0.658699885382972));
#9289=CARTESIAN_POINT('Ctrl Pts',(0.000226633897540712,-7.66527739217044,
-0.66393322296138));
#9290=CARTESIAN_POINT('Ctrl Pts',(-0.0918960199786485,-7.64885315603003,
-0.669166560539789));
#9291=CARTESIAN_POINT('Ctrl Pts',(-0.156516629801222,-7.59769058517097,
-0.674399898118197));
#9292=CARTESIAN_POINT('Ctrl Pts',(-0.215546774837709,-7.55095419585892,
-0.679180488662399));
#9293=CARTESIAN_POINT('Ctrl Pts',(-0.251627560346938,-7.47523005089924,
-0.683961079206601));
#9294=CARTESIAN_POINT('Ctrl Pts',(-0.252073448596348,-7.39987961136196,
-0.688741669750803));
#9295=CARTESIAN_POINT('Ctrl Pts',(-0.252017165498346,-7.40015401716005,
-0.661258330249198));
#9296=CARTESIAN_POINT('Ctrl Pts',(-0.252088041801243,-7.40992057037261,
-0.660639065125953));
#9297=CARTESIAN_POINT('Ctrl Pts',(-0.25156832334334,-7.41967951669182,-0.660019800002709));
#9298=CARTESIAN_POINT('Ctrl Pts',(-0.250432450937044,-7.42936620955704,
-0.659400534879464));
#9299=CARTESIAN_POINT('Ctrl Pts',(-0.240833325255617,-7.51122732506196,
-0.654167197301056));
#9300=CARTESIAN_POINT('Ctrl Pts',(-0.187230064110134,-7.58792828410748,
-0.648933859722648));
#9301=CARTESIAN_POINT('Ctrl Pts',(-0.113656121528127,-7.62508004699099,
-0.643700522144239));
#9302=CARTESIAN_POINT('Ctrl Pts',(-0.0400821789461197,-7.66223180987451,
-0.638467184565831));
#9303=CARTESIAN_POINT('Ctrl Pts',(0.0534624450724112,-7.65983437659602,
-0.633233846987422));
#9304=CARTESIAN_POINT('Ctrl Pts',(0.125036656278963,-7.61896254712631,-0.628000509409014));
#9305=CARTESIAN_POINT('Ctrl Pts',(0.196610867485515,-7.5780907176566,-0.622767171830605));
#9306=CARTESIAN_POINT('Ctrl Pts',(0.246214665880088,-7.49874449199566,-0.617533834252197));
#9307=CARTESIAN_POINT('Ctrl Pts',(0.251607907559673,-7.41649918096761,-0.612300496673789));
#9308=CARTESIAN_POINT('Ctrl Pts',(0.257001149239257,-7.33425386993957,-0.60706715909538));
#9309=CARTESIAN_POINT('Ctrl Pts',(0.218183834203852,-7.24910947354443,-0.601833821516971));
#9310=CARTESIAN_POINT('Ctrl Pts',(0.152559913142665,-7.19924086556578,-0.596600483938563));
#9311=CARTESIAN_POINT('Ctrl Pts',(0.086935992081478,-7.14937225758713,-0.591367146360155));
#9312=CARTESIAN_POINT('Ctrl Pts',(-0.00549453500549198,-7.13477943802497,
-0.586133808781747));
#9313=CARTESIAN_POINT('Ctrl Pts',(-0.0832900084867264,-7.16200517980322,
-0.580900471203338));
#9314=CARTESIAN_POINT('Ctrl Pts',(-0.161085481967961,-7.18923092158147,
-0.57566713362493));
#9315=CARTESIAN_POINT('Ctrl Pts',(-0.22424590184346,-7.25827522470013,-0.570433796046521));
#9316=CARTESIAN_POINT('Ctrl Pts',(-0.244452985661471,-7.33818173858017,
-0.565200458468112));
#9317=CARTESIAN_POINT('Ctrl Pts',(-0.249526797809548,-7.35824552633334,
-0.563886415728474));
#9318=CARTESIAN_POINT('Ctrl Pts',(-0.251892549336989,-7.37899413924599,
-0.562572372988836));
#9319=CARTESIAN_POINT('Ctrl Pts',(-0.251711685022834,-7.3997833335225,-0.561258330249198));
#9320=CARTESIAN_POINT('Origin',(0.,-7.4,-0.45));
#9321=CARTESIAN_POINT('',(-0.251454207353971,-7.40014378921791,-0.461258330249198));
#9322=CARTESIAN_POINT('',(-0.251895011223093,-7.40019827523323,-0.488741669750802));
#9323=CARTESIAN_POINT('',(-0.25175,-7.4,-0.45));
#9324=CARTESIAN_POINT('Ctrl Pts',(-0.251895011223093,-7.40019827523323,
-0.488741669750802));
#9325=CARTESIAN_POINT('Ctrl Pts',(-0.251306428556441,-7.33199055382304,
-0.493061032510774));
#9326=CARTESIAN_POINT('Ctrl Pts',(-0.222557857907552,-7.26334536000167,
-0.497380395270746));
#9327=CARTESIAN_POINT('Ctrl Pts',(-0.173090828377879,-7.21664697959534,
-0.501699758030719));
#9328=CARTESIAN_POINT('Ctrl Pts',(-0.113156602216345,-7.16006724721073,
-0.506933095609127));
#9329=CARTESIAN_POINT('Ctrl Pts',(-0.0228082327120731,-7.13570484976218,
-0.512166433187536));
#9330=CARTESIAN_POINT('Ctrl Pts',(0.0574461554993007,-7.15448278304868,
-0.517399770765944));
#9331=CARTESIAN_POINT('Ctrl Pts',(0.137700543710675,-7.17326071633519,-0.522633108344353));
#9332=CARTESIAN_POINT('Ctrl Pts',(0.20786095062915,-7.23517898035675,-0.527866445922761));
#9333=CARTESIAN_POINT('Ctrl Pts',(0.236470620838672,-7.31247622838102,-0.533099783501169));
#9334=CARTESIAN_POINT('Ctrl Pts',(0.265080291048194,-7.38977347640529,-0.538333121079578));
#9335=CARTESIAN_POINT('Ctrl Pts',(0.252139224548762,-7.48244970843227,-0.543566458657986));
#9336=CARTESIAN_POINT('Ctrl Pts',(0.203449611448168,-7.54895308331631,-0.548799796236395));
#9337=CARTESIAN_POINT('Ctrl Pts',(0.154759998347575,-7.61545645820036,-0.554033133814803));
#9338=CARTESIAN_POINT('Ctrl Pts',(0.0703218386458203,-7.65578697594147,
-0.559266471393212));
#9339=CARTESIAN_POINT('Ctrl Pts',(-0.0120066154728626,-7.65186227152851,
-0.56449980897162));
#9340=CARTESIAN_POINT('Ctrl Pts',(-0.0943350695915468,-7.64793756711556,
-0.569733146550029));
#9341=CARTESIAN_POINT('Ctrl Pts',(-0.174553818127159,-7.59975764054855,
-0.574966484128437));
#9342=CARTESIAN_POINT('Ctrl Pts',(-0.216696396852498,-7.52892416058508,
-0.580199821706846));
#9343=CARTESIAN_POINT('Ctrl Pts',(-0.239624754282723,-7.49038605029967,
-0.583047104388165));
#9344=CARTESIAN_POINT('Ctrl Pts',(-0.251282255013556,-7.44514230351416,
-0.585894387069484));
#9345=CARTESIAN_POINT('Ctrl Pts',(-0.25137527833601,-7.39994331833701,-0.588741669750803));
#9346=CARTESIAN_POINT('Ctrl Pts',(-0.251711685022834,-7.3997833335225,-0.561258330249198));
#9347=CARTESIAN_POINT('Ctrl Pts',(-0.251172234857628,-7.46178967423907,
-0.557339035410427));
#9348=CARTESIAN_POINT('Ctrl Pts',(-0.227977979841335,-7.52415702852661,
-0.553419740571657));
#9349=CARTESIAN_POINT('Ctrl Pts',(-0.186412622838117,-7.56979132243042,
-0.549500445732887));
#9350=CARTESIAN_POINT('Ctrl Pts',(-0.130911428436227,-7.63072566775921,
-0.544267108154479));
#9351=CARTESIAN_POINT('Ctrl Pts',(-0.0426552918719249,-7.66182563377536,
-0.53903377057607));
#9352=CARTESIAN_POINT('Ctrl Pts',(0.038785725966995,-7.64914740004011,-0.533800432997662));
#9353=CARTESIAN_POINT('Ctrl Pts',(0.120226743805915,-7.63646916630487,-0.528567095419253));
#9354=CARTESIAN_POINT('Ctrl Pts',(0.194852642919453,-7.58001273281824,-0.523333757840845));
#9355=CARTESIAN_POINT('Ctrl Pts',(0.229204542838122,-7.50509061308471,-0.518100420262437));
#9356=CARTESIAN_POINT('Ctrl Pts',(0.263556442756791,-7.43016849335117,-0.512867082684028));
#9357=CARTESIAN_POINT('Ctrl Pts',(0.257634343480592,-7.33678068737074,-0.50763374510562));
#9358=CARTESIAN_POINT('Ctrl Pts',(0.214093446943169,-7.26679806554806,-0.502400407527211));
#9359=CARTESIAN_POINT('Ctrl Pts',(0.170552550405746,-7.19681544372539,-0.497167069948803));
#9360=CARTESIAN_POINT('Ctrl Pts',(0.0893928566070999,-7.15023800606048,
-0.491933732370394));
#9361=CARTESIAN_POINT('Ctrl Pts',(0.00700270341056665,-7.14794897033469,
-0.486700394791986));
#9362=CARTESIAN_POINT('Ctrl Pts',(-0.0753874497859666,-7.1456599346089,
-0.481467057213577));
#9363=CARTESIAN_POINT('Ctrl Pts',(-0.159008062380387,-7.18765930082222,
-0.476233719635169));
#9364=CARTESIAN_POINT('Ctrl Pts',(-0.206367431528416,-7.25511645158031,
-0.47100038205676));
#9365=CARTESIAN_POINT('Ctrl Pts',(-0.235754505003739,-7.29697444676534,
-0.46775303145424));
#9366=CARTESIAN_POINT('Ctrl Pts',(-0.251179709674751,-7.34863459471956,
-0.464505680851719));
#9367=CARTESIAN_POINT('Ctrl Pts',(-0.251454207353971,-7.40014378921791,
-0.461258330249198));
#9368=CARTESIAN_POINT('Origin',(0.,-7.4,-0.45));
#9369=CARTESIAN_POINT('',(-0.252147125090441,-7.40001476863366,-0.361258330249198));
#9370=CARTESIAN_POINT('',(-0.251847319535426,-7.39979207600155,-0.388741669750802));
#9371=CARTESIAN_POINT('',(-0.25175,-7.4,-0.45));
#9372=CARTESIAN_POINT('Ctrl Pts',(-0.251847319535426,-7.39979207600155,
-0.388741669750802));
#9373=CARTESIAN_POINT('Ctrl Pts',(-0.251989595225182,-7.38368773667891,
-0.389761002795249));
#9374=CARTESIAN_POINT('Ctrl Pts',(-0.250573880883256,-7.36760829714423,
-0.390780335839695));
#9375=CARTESIAN_POINT('Ctrl Pts',(-0.247508235120279,-7.35184983468962,
-0.391799668884141));
#9376=CARTESIAN_POINT('Ctrl Pts',(-0.231768963975402,-7.27094462496357,
-0.39703300646255));
#9377=CARTESIAN_POINT('Ctrl Pts',(-0.172539514683342,-7.19849997924377,
-0.402266344040958));
#9378=CARTESIAN_POINT('Ctrl Pts',(-0.0963756949442417,-7.16699680195703,
-0.407499681619367));
#9379=CARTESIAN_POINT('Ctrl Pts',(-0.0202118752051417,-7.13549362467028,
-0.412733019197775));
#9380=CARTESIAN_POINT('Ctrl Pts',(0.0728863149809975,-7.14493191581659,
-0.417966356776183));
#9381=CARTESIAN_POINT('Ctrl Pts',(0.141177855474435,-7.19107997225668,-0.423199694354592));
#9382=CARTESIAN_POINT('Ctrl Pts',(0.209469395967872,-7.23722802869677,-0.428433031933));
#9383=CARTESIAN_POINT('Ctrl Pts',(0.252954286768607,-7.32008585043064,-0.433666369511409));
#9384=CARTESIAN_POINT('Ctrl Pts',(0.252135868492745,-7.40250373569222,-0.438899707089817));
#9385=CARTESIAN_POINT('Ctrl Pts',(0.251317450216883,-7.48492162095379,-0.444133044668226));
#9386=CARTESIAN_POINT('Ctrl Pts',(0.206195722864424,-7.56689956974307,-0.449366382246634));
#9387=CARTESIAN_POINT('Ctrl Pts',(0.137001229345556,-7.61168237537139,-0.454599719825043));
#9388=CARTESIAN_POINT('Ctrl Pts',(0.0678067358266871,-7.65646518099971,
-0.459833057403451));
#9389=CARTESIAN_POINT('Ctrl Pts',(-0.0254605238585907,-7.66405284346707,
-0.465066394981859));
#9390=CARTESIAN_POINT('Ctrl Pts',(-0.100983726473419,-7.63104339814856,
-0.470299732560268));
#9391=CARTESIAN_POINT('Ctrl Pts',(-0.176506929088247,-7.59803395283005,
-0.475533070138676));
#9392=CARTESIAN_POINT('Ctrl Pts',(-0.234286074632624,-7.52442739972568,
-0.480766407717085));
#9393=CARTESIAN_POINT('Ctrl Pts',(-0.248415605995416,-7.44322558951315,
-0.485999745295493));
#9394=CARTESIAN_POINT('Ctrl Pts',(-0.25088325415845,-7.42904412144736,-0.48691372011393));
#9395=CARTESIAN_POINT('Ctrl Pts',(-0.252019554996279,-7.41463099210748,
-0.487827694932366));
#9396=CARTESIAN_POINT('Ctrl Pts',(-0.251895011223093,-7.40019827523323,
-0.488741669750802));
#9397=CARTESIAN_POINT('Ctrl Pts',(-0.251454207353971,-7.40014378921791,
-0.461258330249198));
#9398=CARTESIAN_POINT('Ctrl Pts',(-0.25162208230268,-7.43164534292534,-0.45927234327331));
#9399=CARTESIAN_POINT('Ctrl Pts',(-0.246123294961887,-7.46309043707242,
-0.457286356297423));
#9400=CARTESIAN_POINT('Ctrl Pts',(-0.234685910778123,-7.49220240059875,
-0.455300369321535));
#9401=CARTESIAN_POINT('Ctrl Pts',(-0.204546895178166,-7.56891626355623,
-0.450067031743127));
#9402=CARTESIAN_POINT('Ctrl Pts',(-0.133170738276618,-7.62942905416833,
-0.444833694164718));
#9403=CARTESIAN_POINT('Ctrl Pts',(-0.0525592823773014,-7.64660957247344,
-0.43960035658631));
#9404=CARTESIAN_POINT('Ctrl Pts',(0.0280521735220159,-7.66379009077855,
-0.434367019007901));
#9405=CARTESIAN_POINT('Ctrl Pts',(0.117898928419101,-7.63763833677668,-0.429133681429493));
#9406=CARTESIAN_POINT('Ctrl Pts',(0.176697758771395,-7.5798795748334,-0.423900343851084));
#9407=CARTESIAN_POINT('Ctrl Pts',(0.235496589123688,-7.52212081289012,-0.418667006272676));
#9408=CARTESIAN_POINT('Ctrl Pts',(0.263247494931189,-7.43275504300543,-0.413433668694268));
#9409=CARTESIAN_POINT('Ctrl Pts',(0.247508224463957,-7.3518498367627,-0.408200331115859));
#9410=CARTESIAN_POINT('Ctrl Pts',(0.231768953996723,-7.27094463051998,-0.402966993537451));
#9411=CARTESIAN_POINT('Ctrl Pts',(0.172539507254754,-7.19849998791922,-0.397733655959042));
#9412=CARTESIAN_POINT('Ctrl Pts',(0.096375690794842,-7.16699681198883,-0.392500318380634));
#9413=CARTESIAN_POINT('Ctrl Pts',(0.0202118743349312,-7.13549363605845,
-0.387266980802225));
#9414=CARTESIAN_POINT('Ctrl Pts',(-0.072886311842922,-7.14493192679844,
-0.382033643223817));
#9415=CARTESIAN_POINT('Ctrl Pts',(-0.141177849396106,-7.19107998125163,
-0.376800305645409));
#9416=CARTESIAN_POINT('Ctrl Pts',(-0.208781959935431,-7.23676350641753,
-0.371619647180005));
#9417=CARTESIAN_POINT('Ctrl Pts',(-0.252076318944627,-7.3184214692473,-0.366438988714602));
#9418=CARTESIAN_POINT('Ctrl Pts',(-0.252147125090441,-7.40001476863366,
-0.361258330249198));
#9419=CARTESIAN_POINT('Origin',(0.,-7.4,-0.45));
#9420=CARTESIAN_POINT('',(-0.251485858071088,-7.39983751670088,-0.261258330249198));
#9421=CARTESIAN_POINT('',(-0.251389279889816,-7.40008150716695,-0.288741669750802));
#9422=CARTESIAN_POINT('',(-0.25175,-7.4,-0.45));
#9423=CARTESIAN_POINT('Ctrl Pts',(-0.251389279889816,-7.40008150716695,
-0.288741669750802));
#9424=CARTESIAN_POINT('Ctrl Pts',(-0.251250058629027,-7.35321657136339,
-0.291694310658131));
#9425=CARTESIAN_POINT('Ctrl Pts',(-0.238659163200998,-7.30628214770086,
-0.29464695156546));
#9426=CARTESIAN_POINT('Ctrl Pts',(-0.214093456160902,-7.26679805981303,
-0.297599592472789));
#9427=CARTESIAN_POINT('Ctrl Pts',(-0.170552557748908,-7.1968154349772,-0.302832930051197));
#9428=CARTESIAN_POINT('Ctrl Pts',(-0.0893928604558538,-7.15023799530713,
-0.308066267629606));
#9429=CARTESIAN_POINT('Ctrl Pts',(-0.00700270371203047,-7.14794895948283,
-0.313299605208015));
#9430=CARTESIAN_POINT('Ctrl Pts',(0.0753874530317917,-7.14565992365854,
-0.318532942786423));
#9431=CARTESIAN_POINT('Ctrl Pts',(0.159008069226383,-7.18765929168002,-0.323766280364831));
#9432=CARTESIAN_POINT('Ctrl Pts',(0.206367440413426,-7.25511644534241,-0.32899961794324));
#9433=CARTESIAN_POINT('Ctrl Pts',(0.253726811600469,-7.32257359900481,-0.334232955521648));
#9434=CARTESIAN_POINT('Ctrl Pts',(0.264824937779963,-7.41548853830811,-0.339466293100057));
#9435=CARTESIAN_POINT('Ctrl Pts',(0.234685920882397,-7.49220240456848,-0.344699630678465));
#9436=CARTESIAN_POINT('Ctrl Pts',(0.204546903984831,-7.56891627082884,-0.349932968256874));
#9437=CARTESIAN_POINT('Ctrl Pts',(0.133170744010206,-7.62942906404626,-0.355166305835282));
#9438=CARTESIAN_POINT('Ctrl Pts',(0.0525592846402059,-7.64660958309106,
-0.36039964341369));
#9439=CARTESIAN_POINT('Ctrl Pts',(-0.0280521747297935,-7.66379010213587,
-0.365632980992099));
#9440=CARTESIAN_POINT('Ctrl Pts',(-0.117898933495167,-7.63763834700807,
-0.370866318570508));
#9441=CARTESIAN_POINT('Ctrl Pts',(-0.176697766379008,-7.57987958257802,
-0.376099656148916));
#9442=CARTESIAN_POINT('Ctrl Pts',(-0.224043947406287,-7.53337088874017,
-0.380313660682878));
#9443=CARTESIAN_POINT('Ctrl Pts',(-0.251259140426578,-7.46636870597724,
-0.38452766521684));
#9444=CARTESIAN_POINT('Ctrl Pts',(-0.251847319535426,-7.39979207600155,
-0.388741669750802));
#9445=CARTESIAN_POINT('Ctrl Pts',(-0.252147125090441,-7.40001476863366,
-0.361258330249198));
#9446=CARTESIAN_POINT('Ctrl Pts',(-0.252147845077095,-7.40084444360018,
-0.361205651136193));
#9447=CARTESIAN_POINT('Ctrl Pts',(-0.252144095887885,-7.40167411188071,
-0.361152972023188));
#9448=CARTESIAN_POINT('Ctrl Pts',(-0.252135857637182,-7.40250373558439,
-0.361100292910183));
#9449=CARTESIAN_POINT('Ctrl Pts',(-0.251317439396557,-7.48492161729753,
-0.355866955331775));
#9450=CARTESIAN_POINT('Ctrl Pts',(-0.206195713986794,-7.56689956255742,
-0.350633617753366));
#9451=CARTESIAN_POINT('Ctrl Pts',(-0.137001223447051,-7.61168236625759,
-0.345400280174958));
#9452=CARTESIAN_POINT('Ctrl Pts',(-0.067806732907307,-7.65646516995776,
-0.340166942596549));
#9453=CARTESIAN_POINT('Ctrl Pts',(0.025460522762417,-7.6640528320982,-0.334933605018141));
#9454=CARTESIAN_POINT('Ctrl Pts',(0.100983722125631,-7.631043388201,-0.329700267439732));
#9455=CARTESIAN_POINT('Ctrl Pts',(0.176506921488845,-7.59803394430381,-0.324466929861324));
#9456=CARTESIAN_POINT('Ctrl Pts',(0.234286064545549,-7.52442739436897,-0.319233592282915));
#9457=CARTESIAN_POINT('Ctrl Pts',(0.248415595300016,-7.44322558765233,-0.314000254704507));
#9458=CARTESIAN_POINT('Ctrl Pts',(0.262545126054484,-7.36202378093569,-0.308766917126099));
#9459=CARTESIAN_POINT('Ctrl Pts',(0.233025044506715,-7.27322671743724,-0.30353357954769));
#9460=CARTESIAN_POINT('Ctrl Pts',(0.17309082092558,-7.21664698748904,-0.298300241969282));
#9461=CARTESIAN_POINT('Ctrl Pts',(0.113156597344446,-7.16006725754084,-0.293066904390873));
#9462=CARTESIAN_POINT('Ctrl Pts',(0.0228082317299446,-7.13570486114289,
-0.287833566812465));
#9463=CARTESIAN_POINT('Ctrl Pts',(-0.0574461530260513,-7.15448279362015,
-0.282600229234056));
#9464=CARTESIAN_POINT('Ctrl Pts',(-0.137700537782047,-7.17326072609741,
-0.277366891655648));
#9465=CARTESIAN_POINT('Ctrl Pts',(-0.207860941679538,-7.23517898744989,
-0.272133554077239));
#9466=CARTESIAN_POINT('Ctrl Pts',(-0.236470610657442,-7.31247623214764,
-0.266900216498831));
#9467=CARTESIAN_POINT('Ctrl Pts',(-0.246751653146716,-7.34025342375566,
-0.265019587748953));
#9468=CARTESIAN_POINT('Ctrl Pts',(-0.251666983719407,-7.37001660175744,
-0.263138958999076));
#9469=CARTESIAN_POINT('Ctrl Pts',(-0.251485858071088,-7.39983751670088,
-0.261258330249198));
#9470=CARTESIAN_POINT('Origin',(0.,-7.4,-0.45));
#9471=CARTESIAN_POINT('',(-0.2516645197469,-7.40021351101923,-0.161258330249198));
#9472=CARTESIAN_POINT('',(-0.252102603566075,-7.4000936994049,-0.188741669750802));
#9473=CARTESIAN_POINT('',(-0.25175,-7.4,-0.45));
#9474=CARTESIAN_POINT('Ctrl Pts',(-0.252102603566075,-7.4000936994049,-0.188741669750802));
#9475=CARTESIAN_POINT('Ctrl Pts',(-0.2517296574347,-7.32310553688027,-0.193627618521014));
#9476=CARTESIAN_POINT('Ctrl Pts',(-0.213827729289536,-7.24579919004338,
-0.198513567291226));
#9477=CARTESIAN_POINT('Ctrl Pts',(-0.152559919713999,-7.19924085691687,
-0.203399516061437));
#9478=CARTESIAN_POINT('Ctrl Pts',(-0.0869359958298059,-7.14937224678642,
-0.208632853639846));
#9479=CARTESIAN_POINT('Ctrl Pts',(0.00549453524232928,-7.13477942660635,
-0.213866191218254));
#9480=CARTESIAN_POINT('Ctrl Pts',(0.0832900120743056,-7.16200516955927,
-0.219099528796662));
#9481=CARTESIAN_POINT('Ctrl Pts',(0.161085488906282,-7.18923091251219,-0.224332866375071));
#9482=CARTESIAN_POINT('Ctrl Pts',(0.224245911498099,-7.2582752185981,-0.229566203953479));
#9483=CARTESIAN_POINT('Ctrl Pts',(0.244452996185411,-7.33818173591718,-0.234799541531888));
#9484=CARTESIAN_POINT('Ctrl Pts',(0.264660080872723,-7.41808825323625,-0.240032879110296));
#9485=CARTESIAN_POINT('Ctrl Pts',(0.241913827655531,-7.50885698178848,-0.245266216688705));
#9486=CARTESIAN_POINT('Ctrl Pts',(0.186412630864449,-7.56979132974143,-0.250499554267113));
#9487=CARTESIAN_POINT('Ctrl Pts',(0.130911434073366,-7.63072567769439,-0.255732891845521));
#9488=CARTESIAN_POINT('Ctrl Pts',(0.0426552937083935,-7.66182564504807,
-0.26096622942393));
#9489=CARTESIAN_POINT('Ctrl Pts',(-0.0387857276371238,-7.64914741076662,
-0.266199567002338));
#9490=CARTESIAN_POINT('Ctrl Pts',(-0.120226748982641,-7.63646917648517,
-0.271432904580747));
#9491=CARTESIAN_POINT('Ctrl Pts',(-0.194852651308702,-7.5800127405686,-0.276666242159156));
#9492=CARTESIAN_POINT('Ctrl Pts',(-0.229204552706265,-7.50509061760952,
-0.281899579737564));
#9493=CARTESIAN_POINT('Ctrl Pts',(-0.244175164861291,-7.47243943968284,
-0.284180276408643));
#9494=CARTESIAN_POINT('Ctrl Pts',(-0.251496818014495,-7.43628120311108,
-0.286460973079723));
#9495=CARTESIAN_POINT('Ctrl Pts',(-0.251389279889816,-7.40008150716695,
-0.288741669750802));
#9496=CARTESIAN_POINT('Ctrl Pts',(-0.251485858071088,-7.39983751670088,
-0.261258330249198));
#9497=CARTESIAN_POINT('Ctrl Pts',(-0.251162954595198,-7.453001037046,-0.257905621420667));
#9498=CARTESIAN_POINT('Ctrl Pts',(-0.234642333184093,-7.5063480587605,-0.254552912592136));
#9499=CARTESIAN_POINT('Ctrl Pts',(-0.20344960268904,-7.54895307690641,-0.251200203763606));
#9500=CARTESIAN_POINT('Ctrl Pts',(-0.154759991684416,-7.61545644892441,
-0.245966866185197));
#9501=CARTESIAN_POINT('Ctrl Pts',(-0.0703218356168507,-7.65578696491737,
-0.240733528606789));
#9502=CARTESIAN_POINT('Ctrl Pts',(0.0120066149565192,-7.65186226067865,
-0.23550019102838));
#9503=CARTESIAN_POINT('Ctrl Pts',(0.0943350655298891,-7.64793755643993,
-0.230266853449972));
#9504=CARTESIAN_POINT('Ctrl Pts',(0.174553810609064,-7.59975763196954,-0.225033515871563));
#9505=CARTESIAN_POINT('Ctrl Pts',(0.216696387521491,-7.52892415504588,-0.219800178293155));
#9506=CARTESIAN_POINT('Ctrl Pts',(0.258838964433917,-7.45809067812223,-0.214566840714747));
#9507=CARTESIAN_POINT('Ctrl Pts',(0.262905373179595,-7.36460364874532,-0.209333503136338));
#9508=CARTESIAN_POINT('Ctrl Pts',(0.227072427000858,-7.29037849046193,-0.20410016555793));
#9509=CARTESIAN_POINT('Ctrl Pts',(0.191239480822121,-7.21615333217855,-0.198866827979521));
#9510=CARTESIAN_POINT('Ctrl Pts',(0.115507179718968,-7.1611900449887,-0.193633490401113));
#9511=CARTESIAN_POINT('Ctrl Pts',(0.0338304498224533,-7.15013155025275,
-0.188400152822704));
#9512=CARTESIAN_POINT('Ctrl Pts',(-0.0478462800740612,-7.13907305551679,
-0.183166815244296));
#9513=CARTESIAN_POINT('Ctrl Pts',(-0.135467438763938,-7.17191935323474,
-0.177933477665887));
#9514=CARTESIAN_POINT('Ctrl Pts',(-0.189747630523594,-7.23394391472528,
-0.172700140087479));
#9515=CARTESIAN_POINT('Ctrl Pts',(-0.229305791562914,-7.27914599512138,
-0.168886203474719));
#9516=CARTESIAN_POINT('Ctrl Pts',(-0.251156029290448,-7.33984512028938,
-0.165072266861958));
#9517=CARTESIAN_POINT('Ctrl Pts',(-0.2516645197469,-7.40021351101923,-0.161258330249198));
#9518=CARTESIAN_POINT('Origin',(0.,-7.4,-0.45));
#9519=CARTESIAN_POINT('',(-0.25205356191611,-7.39987360404796,-0.0612583302491979));
#9520=CARTESIAN_POINT('',(-0.251593604700942,-7.39979879766985,-0.0887416697508022));
#9521=CARTESIAN_POINT('',(-0.25175,-7.4,-0.45));
#9522=CARTESIAN_POINT('',(0.191346599666505,-7.2364012796625,0.));
#9523=CARTESIAN_POINT('Ctrl Pts',(-0.25205356191611,-7.39987360404796,-0.0612583302491979));
#9524=CARTESIAN_POINT('Ctrl Pts',(-0.251574539177045,-7.47426199643967,
-0.056538899568024));
#9525=CARTESIAN_POINT('Ctrl Pts',(-0.216528582359325,-7.54902721912311,
-0.0518194688868501));
#9526=CARTESIAN_POINT('Ctrl Pts',(-0.158787390485525,-7.59585256738247,
-0.0471000382056762));
#9527=CARTESIAN_POINT('Ctrl Pts',(-0.094758661244801,-7.64777680808492,
-0.0418667006272677));
#9528=CARTESIAN_POINT('Ctrl Pts',(-0.00282294424260245,-7.66534503829956,
-0.0366333630488592));
#9529=CARTESIAN_POINT('Ctrl Pts',(0.0757847404228917,-7.64053050058079,
-0.0314000254704507));
#9530=CARTESIAN_POINT('Ctrl Pts',(0.154392425088386,-7.61571596286203,-0.0261666878920423));
#9531=CARTESIAN_POINT('Ctrl Pts',(0.219672077417175,-7.54851865720985,-0.0209333503136338));
#9532=CARTESIAN_POINT('Ctrl Pts',(0.242359266047042,-7.46941964788139,-0.0157000127352254));
#9533=CARTESIAN_POINT('Ctrl Pts',(0.265046454676908,-7.39032063855293,-0.0104666751568169));
#9534=CARTESIAN_POINT('Ctrl Pts',(0.245141179607852,-7.29931992554818,-0.00523333757840846));
#9535=CARTESIAN_POINT('Ctrl Pts',(0.191346599666505,-7.2364012796625,0.));
#9536=CARTESIAN_POINT('',(-0.191702382984482,-7.23617294784579,6.20293008155665E-17));
#9537=CARTESIAN_POINT('Origin',(0.,-7.4,0.));
#9538=CARTESIAN_POINT('Ctrl Pts',(-0.191704050234201,-7.23617187785139,
3.46944695195361E-17));
#9539=CARTESIAN_POINT('Ctrl Pts',(-0.14033257538867,-7.17646167822941,-0.00499978774624427));
#9540=CARTESIAN_POINT('Ctrl Pts',(-0.0585928813496691,-7.14242247150708,
-0.00999957549248857));
#9541=CARTESIAN_POINT('Ctrl Pts',(0.0199179744619951,-7.14865372872736,
-0.0149993632387329));
#9542=CARTESIAN_POINT('Ctrl Pts',(0.102096225396913,-7.15517606011955,-0.0202327008171413));
#9543=CARTESIAN_POINT('Ctrl Pts',(0.180736942103683,-7.2058189496042,-0.0254660383955497));
#9544=CARTESIAN_POINT('Ctrl Pts',(0.220629131202208,-7.27793230733172,-0.0306993759739582));
#9545=CARTESIAN_POINT('Ctrl Pts',(0.260521320300732,-7.35004566505924,-0.0359327135523667));
#9546=CARTESIAN_POINT('Ctrl Pts',(0.261664981791011,-7.44362949102963,-0.0411660511307752));
#9547=CARTESIAN_POINT('Ctrl Pts',(0.223523601724647,-7.51669742191632,-0.0463993887091836));
#9548=CARTESIAN_POINT('Ctrl Pts',(0.185382221658284,-7.58976535280302,-0.0516327262875921));
#9549=CARTESIAN_POINT('Ctrl Pts',(0.107955800035278,-7.64231738860601,-0.0568660638660005));
#9550=CARTESIAN_POINT('Ctrl Pts',(0.0259706150012631,-7.6508052506037,-0.0620994014444089));
#9551=CARTESIAN_POINT('Ctrl Pts',(-0.0560145700327524,-7.65929311260139,
-0.0673327390228174));
#9552=CARTESIAN_POINT('Ctrl Pts',(-0.142558518477778,-7.62371680079378,
-0.0725660766012259));
#9553=CARTESIAN_POINT('Ctrl Pts',(-0.194864670716722,-7.56002034494844,
-0.0777994141796343));
#9554=CARTESIAN_POINT('Ctrl Pts',(-0.231319882275806,-7.51562656574637,
-0.081446832703357));
#9555=CARTESIAN_POINT('Ctrl Pts',(-0.25114405026367,-7.45757339860048,-0.0850942512270796));
#9556=CARTESIAN_POINT('Ctrl Pts',(-0.251593604700942,-7.39979879766985,
-0.0887416697508022));
#9557=CARTESIAN_POINT('Origin',(0.,7.4,-0.45));
#9558=CARTESIAN_POINT('',(-0.251358460963395,7.39999011478219,-0.761258330249198));
#9559=CARTESIAN_POINT('',(-0.2515844849848,7.39966621586329,-0.788741669750802));
#9560=CARTESIAN_POINT('',(-0.25175,7.4,-0.45));
#9561=CARTESIAN_POINT('',(-0.191346599666504,7.5635987203375,-0.8));
#9562=CARTESIAN_POINT('Ctrl Pts',(-0.2515844849848,7.39966621586329,-0.788741669750802));
#9563=CARTESIAN_POINT('Ctrl Pts',(-0.251071187758555,7.45892160063636,-0.792494446500535));
#9564=CARTESIAN_POINT('Ctrl Pts',(-0.229922182808404,7.51848035603044,-0.796247223250268));
#9565=CARTESIAN_POINT('Ctrl Pts',(-0.191346599666504,7.5635987203375,-0.8));
#9566=CARTESIAN_POINT('',(0.191702360493801,7.56382706695207,-0.8));
#9567=CARTESIAN_POINT('Origin',(0.,7.4,-0.8));
#9568=CARTESIAN_POINT('Ctrl Pts',(0.191704026215797,7.56382813610288,-0.8));
#9569=CARTESIAN_POINT('Ctrl Pts',(0.140332545101572,7.62353836531877,-0.795000212253756));
#9570=CARTESIAN_POINT('Ctrl Pts',(0.058592868207462,7.65757749184722,-0.790000424507511));
#9571=CARTESIAN_POINT('Ctrl Pts',(-0.0199179742868679,7.65134621809807,
-0.785000636761267));
#9572=CARTESIAN_POINT('Ctrl Pts',(-0.102096211282372,7.64482386940491,-0.779767299182859));
#9573=CARTESIAN_POINT('Ctrl Pts',(-0.18073691824322,7.59418103237105,-0.774533961604451));
#9574=CARTESIAN_POINT('Ctrl Pts',(-0.220629103980957,7.52206769300185,-0.769300624026042));
#9575=CARTESIAN_POINT('Ctrl Pts',(-0.241063780214276,7.48512780828857,-0.766619859433761));
#9576=CARTESIAN_POINT('Ctrl Pts',(-0.251330937500274,7.44255411530564,-0.763939094841479));
#9577=CARTESIAN_POINT('Ctrl Pts',(-0.251358460963395,7.39999011478219,-0.761258330249198));
#9578=CARTESIAN_POINT('Origin',(0.,7.4,-0.45));
#9579=CARTESIAN_POINT('',(-0.252017148126658,7.3998459827829,-0.661258330249197));
#9580=CARTESIAN_POINT('',(-0.252073462769148,7.40012038728064,-0.688741669750802));
#9581=CARTESIAN_POINT('',(-0.25175,7.4,-0.45));
#9582=CARTESIAN_POINT('Ctrl Pts',(-0.252073462769148,7.40012038728064,-0.688741669750802));
#9583=CARTESIAN_POINT('Ctrl Pts',(-0.252115690748467,7.40725647012215,-0.689194416785009));
#9584=CARTESIAN_POINT('Ctrl Pts',(-0.251838306299564,7.41438920118803,-0.689647163819216));
#9585=CARTESIAN_POINT('Ctrl Pts',(-0.251230534080426,7.42149364028408,-0.690099910853423));
#9586=CARTESIAN_POINT('Ctrl Pts',(-0.244205248538583,7.50361439489039,-0.695333248431831));
#9587=CARTESIAN_POINT('Ctrl Pts',(-0.193036110221656,7.58195499579916,-0.700566586010239));
#9588=CARTESIAN_POINT('Ctrl Pts',(-0.120664077269321,7.62139994469436,-0.705799923588648));
#9589=CARTESIAN_POINT('Ctrl Pts',(-0.0482920443169851,7.66084489358957,
-0.711033261167056));
#9590=CARTESIAN_POINT('Ctrl Pts',(0.0452828832707578,7.6613941904712,-0.716266598745465));
#9591=CARTESIAN_POINT('Ctrl Pts',(0.118103980273902,7.62278362739801,-0.721499936323873));
#9592=CARTESIAN_POINT('Ctrl Pts',(0.190925077277045,7.58417306432483,-0.726733273902282));
#9593=CARTESIAN_POINT('Ctrl Pts',(0.242992343695589,7.50640264129683,-0.73196661148069));
#9594=CARTESIAN_POINT('Ctrl Pts',(0.250965115890772,7.42437728229464,-0.737199949059099));
#9595=CARTESIAN_POINT('Ctrl Pts',(0.258937888085954,7.34235192329245,-0.742433286637507));
#9596=CARTESIAN_POINT('Ctrl Pts',(0.222816166057774,7.25607162831608,-0.747666624215915));
#9597=CARTESIAN_POINT('Ctrl Pts',(0.158787417691483,7.20414739331457,-0.752899961794324));
#9598=CARTESIAN_POINT('Ctrl Pts',(0.0947586693251928,7.15222315831307,-0.758133299372733));
#9599=CARTESIAN_POINT('Ctrl Pts',(0.00282289462079141,7.13465498328644,
-0.763366636951141));
#9600=CARTESIAN_POINT('Ctrl Pts',(-0.0757847619957929,7.15946949434078,
-0.76859997452955));
#9601=CARTESIAN_POINT('Ctrl Pts',(-0.154392418612378,7.18428400539513,-0.773833312107958));
#9602=CARTESIAN_POINT('Ctrl Pts',(-0.219671957141145,7.25148120253045,-0.779066649686367));
#9603=CARTESIAN_POINT('Ctrl Pts',(-0.242359147390014,7.33058021979462,-0.784299987264775));
#9604=CARTESIAN_POINT('Ctrl Pts',(-0.24877756865406,7.3529580818747,-0.785780548093451));
#9605=CARTESIAN_POINT('Ctrl Pts',(-0.251786993105406,7.37628853916314,-0.787261108922127));
#9606=CARTESIAN_POINT('Ctrl Pts',(-0.2515844849848,7.39966621586329,-0.788741669750802));
#9607=CARTESIAN_POINT('Ctrl Pts',(-0.251358460963395,7.39999011478219,-0.761258330249198));
#9608=CARTESIAN_POINT('Ctrl Pts',(-0.25138466828076,7.35946148417043,-0.758705757263071));
#9609=CARTESIAN_POINT('Ctrl Pts',(-0.242127126249713,7.31894164121318,-0.756153184276943));
#9610=CARTESIAN_POINT('Ctrl Pts',(-0.223523578567029,7.28330258339987,-0.753600611290816));
#9611=CARTESIAN_POINT('Ctrl Pts',(-0.185382202900737,7.21023465487163,-0.748367273712408));
#9612=CARTESIAN_POINT('Ctrl Pts',(-0.107955787053529,7.15768263951967,-0.743133936134));
#9613=CARTESIAN_POINT('Ctrl Pts',(-0.025970610812802,7.14919478175684,-0.737900598555592));
#9614=CARTESIAN_POINT('Ctrl Pts',(0.0560145654279252,7.14070692399402,-0.732667260977183));
#9615=CARTESIAN_POINT('Ctrl Pts',(0.14255850206217,7.17628322382034,-0.727433923398774));
#9616=CARTESIAN_POINT('Ctrl Pts',(0.194864648070335,7.2399796707009,-0.722200585820366));
#9617=CARTESIAN_POINT('Ctrl Pts',(0.247170794078499,7.30367611758145,-0.716967248241957));
#9618=CARTESIAN_POINT('Ctrl Pts',(0.265239149460586,7.39549271151625,-0.711733910663549));
#9619=CARTESIAN_POINT('Ctrl Pts',(0.240965785765977,7.47425967354379,-0.706500573085141));
#9620=CARTESIAN_POINT('Ctrl Pts',(0.216692422071369,7.55302663557132,-0.701267235506732));
#9621=CARTESIAN_POINT('Ctrl Pts',(0.150077339300067,7.61874396569159,-0.696033897928324));
#9622=CARTESIAN_POINT('Ctrl Pts',(0.0709891645753919,7.64194865395628,-0.690800560349915));
#9623=CARTESIAN_POINT('Ctrl Pts',(-0.00809901014928227,7.66515334222097,
-0.685567222771507));
#9624=CARTESIAN_POINT('Ctrl Pts',(-0.0996602768273276,7.64584538863009,
-0.680333885193098));
#9625=CARTESIAN_POINT('Ctrl Pts',(-0.162643413958381,7.59268077865113,-0.67510054761469));
#9626=CARTESIAN_POINT('Ctrl Pts',(-0.21817370487162,7.54580718052792,-0.670486475159526));
#9627=CARTESIAN_POINT('Ctrl Pts',(-0.251489057009901,7.47261543070241,-0.665872402704361));
#9628=CARTESIAN_POINT('Ctrl Pts',(-0.252017148126658,7.3998459827829,-0.661258330249197));
#9629=CARTESIAN_POINT('Origin',(0.,7.4,-0.45));
#9630=CARTESIAN_POINT('',(-0.251711667638598,7.40021666645972,-0.561258330249198));
#9631=CARTESIAN_POINT('',(-0.251375292868799,7.40005668164188,-0.588741669750802));
#9632=CARTESIAN_POINT('',(-0.25175,7.4,-0.45));
#9633=CARTESIAN_POINT('Ctrl Pts',(-0.251375292868799,7.40005668164188,-0.588741669750802));
#9634=CARTESIAN_POINT('Ctrl Pts',(-0.251453247461991,7.4379339415428,-0.591127724647892));
#9635=CARTESIAN_POINT('Ctrl Pts',(-0.243409898811809,7.47577976703267,-0.593513779544981));
#9636=CARTESIAN_POINT('Ctrl Pts',(-0.227072449902118,7.50962152054577,-0.595899834442071));
#9637=CARTESIAN_POINT('Ctrl Pts',(-0.191239500115965,7.58384668636041,-0.601133172020479));
#9638=CARTESIAN_POINT('Ctrl Pts',(-0.115507191401049,7.63880997927991,-0.606366509598887));
#9639=CARTESIAN_POINT('Ctrl Pts',(-0.0338304532489083,7.64986847505112,
-0.611599847177296));
#9640=CARTESIAN_POINT('Ctrl Pts',(0.0478462849032329,7.66092697082232,-0.616833184755704));
#9641=CARTESIAN_POINT('Ctrl Pts',(0.135467452492599,7.62808066944522,-0.622066522334113));
#9642=CARTESIAN_POINT('Ctrl Pts',(0.189747649694627,7.56605610184571,-0.627299859912522));
#9643=CARTESIAN_POINT('Ctrl Pts',(0.244027846896655,7.5040315342462,-0.63253319749093));
#9644=CARTESIAN_POINT('Ctrl Pts',(0.264967073711345,7.41282870042428,-0.637766535069338));
#9645=CARTESIAN_POINT('Ctrl Pts',(0.243177185935535,7.33333936475981,-0.642999872647746));
#9646=CARTESIAN_POINT('Ctrl Pts',(0.221387298159724,7.25385002909535,-0.648233210226155));
#9647=CARTESIAN_POINT('Ctrl Pts',(0.156868295793411,7.18607419158834,-0.653466547804564));
#9648=CARTESIAN_POINT('Ctrl Pts',(0.0785474648464412,7.16039839199962,-0.658699885382972));
#9649=CARTESIAN_POINT('Ctrl Pts',(0.000226633899471557,7.1347225924109,
-0.663933222961381));
#9650=CARTESIAN_POINT('Ctrl Pts',(-0.0918960256281538,7.15114683074047,
-0.669166560539789));
#9651=CARTESIAN_POINT('Ctrl Pts',(-0.156516639008589,7.20230940405719,-0.674399898118197));
#9652=CARTESIAN_POINT('Ctrl Pts',(-0.215546787295137,7.24904579561427,-0.679180488662399));
#9653=CARTESIAN_POINT('Ctrl Pts',(-0.251627574307423,7.32476994304303,-0.6839610792066));
#9654=CARTESIAN_POINT('Ctrl Pts',(-0.252073462769148,7.40012038728064,-0.688741669750802));
#9655=CARTESIAN_POINT('Ctrl Pts',(-0.252017148126658,7.3998459827829,-0.661258330249197));
#9656=CARTESIAN_POINT('Ctrl Pts',(-0.252088024432499,7.39007943022609,-0.660639065125953));
#9657=CARTESIAN_POINT('Ctrl Pts',(-0.251568306017017,7.38032048456503,-0.660019800002709));
#9658=CARTESIAN_POINT('Ctrl Pts',(-0.250432433693752,7.37063379235739,-0.659400534879464));
#9659=CARTESIAN_POINT('Ctrl Pts',(-0.240833308714009,7.28877268240962,-0.654167197301056));
#9660=CARTESIAN_POINT('Ctrl Pts',(-0.187230051170462,7.21207172888109,-0.648933859722647));
#9661=CARTESIAN_POINT('Ctrl Pts',(-0.113656113647963,7.17491996861538,-0.643700522144239));
#9662=CARTESIAN_POINT('Ctrl Pts',(-0.0400821761254621,7.13776820834967,
-0.638467184565831));
#9663=CARTESIAN_POINT('Ctrl Pts',(0.0534624413759923,7.14016564134677,-0.633233846987422));
#9664=CARTESIAN_POINT('Ctrl Pts',(0.125036647626303,7.18103746796602,-0.628000509409014));
#9665=CARTESIAN_POINT('Ctrl Pts',(0.196610853876614,7.22190929458527,-0.622767171830605));
#9666=CARTESIAN_POINT('Ctrl Pts',(0.246214648875781,7.30125551482666,-0.617533834252197));
#9667=CARTESIAN_POINT('Ctrl Pts',(0.251607890189855,7.38350082018848,-0.612300496673788));
#9668=CARTESIAN_POINT('Ctrl Pts',(0.257001131503928,7.46574612555029,-0.60706715909538));
#9669=CARTESIAN_POINT('Ctrl Pts',(0.218183819132908,7.55089051603252,-0.601833821516972));
#9670=CARTESIAN_POINT('Ctrl Pts',(0.152559902600542,7.6007591205591,-0.596600483938563));
#9671=CARTESIAN_POINT('Ctrl Pts',(0.0869359860681766,7.65062772508569,-0.591367146360155));
#9672=CARTESIAN_POINT('Ctrl Pts',(-0.00549453462553363,7.66522054365662,
-0.586133808781746));
#9673=CARTESIAN_POINT('Ctrl Pts',(-0.0832900027313079,7.63799480376286,
-0.580900471203338));
#9674=CARTESIAN_POINT('Ctrl Pts',(-0.161085470837084,7.61076906386911,-0.575667133624929));
#9675=CARTESIAN_POINT('Ctrl Pts',(-0.224245886354923,7.54172476551065,-0.570433796046521));
#9676=CARTESIAN_POINT('Ctrl Pts',(-0.244452968778356,7.46181825714769,-0.565200458468112));
#9677=CARTESIAN_POINT('Ctrl Pts',(-0.249526780576268,7.44175447077981,-0.563886415728474));
#9678=CARTESIAN_POINT('Ctrl Pts',(-0.251892531940355,7.42100585930017,-0.562572372988836));
#9679=CARTESIAN_POINT('Ctrl Pts',(-0.251711667638598,7.40021666645972,-0.561258330249198));
#9680=CARTESIAN_POINT('Origin',(0.,7.4,-0.45));
#9681=CARTESIAN_POINT('',(-0.251454189985941,7.399856210792,-0.461258330249197));
#9682=CARTESIAN_POINT('',(-0.251895025789683,7.3998017247554,-0.488741669750802));
#9683=CARTESIAN_POINT('',(-0.25175,7.4,-0.45));
#9684=CARTESIAN_POINT('Ctrl Pts',(-0.251895025789683,7.3998017247554,-0.488741669750802));
#9685=CARTESIAN_POINT('Ctrl Pts',(-0.251306443088966,7.46800945010948,-0.493061032510774));
#9686=CARTESIAN_POINT('Ctrl Pts',(-0.222557870777557,7.53665464789974,-0.497380395270746));
#9687=CARTESIAN_POINT('Ctrl Pts',(-0.17309083838734,7.583353031007,-0.501699758030719));
#9688=CARTESIAN_POINT('Ctrl Pts',(-0.113156608759973,7.63993276666405,-0.506933095609127));
#9689=CARTESIAN_POINT('Ctrl Pts',(-0.0228082340311984,7.66429516552368,
-0.512166433187536));
#9690=CARTESIAN_POINT('Ctrl Pts',(0.0574461588212237,7.64551723115025,-0.517399770765944));
#9691=CARTESIAN_POINT('Ctrl Pts',(0.137700551673646,7.62673929677682,-0.522633108344352));
#9692=CARTESIAN_POINT('Ctrl Pts',(0.207860962649715,7.56482102917033,-0.527866445922761));
#9693=CARTESIAN_POINT('Ctrl Pts',(0.236470634513469,7.48752377667808,-0.533099783501169));
#9694=CARTESIAN_POINT('Ctrl Pts',(0.265080306377223,7.41022652418583,-0.538333121079578));
#9695=CARTESIAN_POINT('Ctrl Pts',(0.252139239128661,7.31755028680782,-0.543566458657986));
#9696=CARTESIAN_POINT('Ctrl Pts',(0.203449623212889,7.25104690807429,-0.548799796236395));
#9697=CARTESIAN_POINT('Ctrl Pts',(0.154760007297116,7.18454352934075,-0.554033133814803));
#9698=CARTESIAN_POINT('Ctrl Pts',(0.0703218427141316,7.1442130092517,-0.559266471393212));
#9699=CARTESIAN_POINT('Ctrl Pts',(-0.0120066161663935,7.14813771389866,
-0.56449980897162));
#9700=CARTESIAN_POINT('Ctrl Pts',(-0.0943350750469181,7.15206241854562,
-0.569733146550028));
#9701=CARTESIAN_POINT('Ctrl Pts',(-0.174553828224984,7.20024234792858,-0.574966484128437));
#9702=CARTESIAN_POINT('Ctrl Pts',(-0.216696409385322,7.27107583197496,-0.580199821706845));
#9703=CARTESIAN_POINT('Ctrl Pts',(-0.239624768140347,7.30961394448175,-0.583047104388164));
#9704=CARTESIAN_POINT('Ctrl Pts',(-0.251282269542556,7.35485769386367,-0.585894387069483));
#9705=CARTESIAN_POINT('Ctrl Pts',(-0.251375292868799,7.40005668164188,-0.588741669750802));
#9706=CARTESIAN_POINT('Ctrl Pts',(-0.251711667638598,7.40021666645972,-0.561258330249198));
#9707=CARTESIAN_POINT('Ctrl Pts',(-0.251172217510369,7.33821033002641,-0.557339035410427));
#9708=CARTESIAN_POINT('Ctrl Pts',(-0.227977964094547,7.27584298004936,-0.553419740571657));
#9709=CARTESIAN_POINT('Ctrl Pts',(-0.18641260996181,7.23020868929834,-0.549500445732887));
#9710=CARTESIAN_POINT('Ctrl Pts',(-0.130911419392803,7.1692743481794,-0.544267108154479));
#9711=CARTESIAN_POINT('Ctrl Pts',(-0.0426552889257632,7.13817438430899,
-0.53903377057607));
#9712=CARTESIAN_POINT('Ctrl Pts',(0.0387857232876696,7.15085261716797,-0.533800432997662));
#9713=CARTESIAN_POINT('Ctrl Pts',(0.120226735501102,7.16353085002696,-0.528567095419254));
#9714=CARTESIAN_POINT('Ctrl Pts',(0.194852629460927,7.21998727961534,-0.523333757840845));
#9715=CARTESIAN_POINT('Ctrl Pts',(0.22920452700707,7.29490939417427,-0.518100420262437));
#9716=CARTESIAN_POINT('Ctrl Pts',(0.263556424553213,7.36983150873319,-0.512867082684028));
#9717=CARTESIAN_POINT('Ctrl Pts',(0.257634325685674,7.46321930826266,-0.50763374510562));
#9718=CARTESIAN_POINT('Ctrl Pts',(0.214093432155548,7.53320192525145,-0.502400407527211));
#9719=CARTESIAN_POINT('Ctrl Pts',(0.170552538625422,7.60318454224025,-0.497167069948803));
#9720=CARTESIAN_POINT('Ctrl Pts',(0.0893928504327086,7.64976197668837,-0.491933732370394));
#9721=CARTESIAN_POINT('Ctrl Pts',(0.00700270292694295,7.65205101225613,
-0.486700394791986));
#9722=CARTESIAN_POINT('Ctrl Pts',(-0.0753874445788215,7.6543400478239,-0.481467057213577));
#9723=CARTESIAN_POINT('Ctrl Pts',(-0.159008051397638,7.61234068451132,-0.476233719635169));
#9724=CARTESIAN_POINT('Ctrl Pts',(-0.206367417274562,7.54488353841248,-0.47100038205676));
#9725=CARTESIAN_POINT('Ctrl Pts',(-0.235754488720125,7.50302554611858,-0.467753031454239));
#9726=CARTESIAN_POINT('Ctrl Pts',(-0.251179692325698,7.45136540173257,-0.464505680851719));
#9727=CARTESIAN_POINT('Ctrl Pts',(-0.251454189985941,7.399856210792,-0.461258330249197));
#9728=CARTESIAN_POINT('Origin',(0.,7.4,-0.45));
#9729=CARTESIAN_POINT('',(-0.252147107674537,7.3999852313674,-0.361258330249197));
#9730=CARTESIAN_POINT('',(-0.251847334099258,7.40020792401048,-0.388741669750802));
#9731=CARTESIAN_POINT('',(-0.25175,7.4,-0.45));
#9732=CARTESIAN_POINT('Ctrl Pts',(-0.251847334099258,7.40020792401048,-0.388741669750802));
#9733=CARTESIAN_POINT('Ctrl Pts',(-0.251989609797241,7.41631226426441,-0.389761002795248));
#9734=CARTESIAN_POINT('Ctrl Pts',(-0.250573895373447,7.43239170472893,-0.390780335839695));
#9735=CARTESIAN_POINT('Ctrl Pts',(-0.24750824943319,7.44815016809482,-0.391799668884141));
#9736=CARTESIAN_POINT('Ctrl Pts',(-0.231768977378143,7.52905538249945,-0.39703300646255));
#9737=CARTESIAN_POINT('Ctrl Pts',(-0.172539524660956,7.60150003240856,-0.402266344040958));
#9738=CARTESIAN_POINT('Ctrl Pts',(-0.0963757005174525,7.63300321151708,
-0.407499681619367));
#9739=CARTESIAN_POINT('Ctrl Pts',(-0.0202118763739491,7.66450639062559,
-0.412733019197775));
#9740=CARTESIAN_POINT('Ctrl Pts',(0.0728863191958706,7.65506809893352,-0.417966356776183));
#9741=CARTESIAN_POINT('Ctrl Pts',(0.141177863638472,7.60892003982476,-0.423199694354592));
#9742=CARTESIAN_POINT('Ctrl Pts',(0.209469408081073,7.562771980716,-0.428433031933));
#9743=CARTESIAN_POINT('Ctrl Pts',(0.252954301396456,7.47991415419055,-0.433666369511409));
#9744=CARTESIAN_POINT('Ctrl Pts',(0.252135883073263,7.39749626416295,-0.438899707089817));
#9745=CARTESIAN_POINT('Ctrl Pts',(0.251317464750071,7.31507837413536,-0.444133044668226));
#9746=CARTESIAN_POINT('Ctrl Pts',(0.206195734788304,7.23310042060562,-0.449366382246634));
#9747=CARTESIAN_POINT('Ctrl Pts',(0.13700123726806,7.18831761238753,-0.454599719825042));
#9748=CARTESIAN_POINT('Ctrl Pts',(0.0678067397478142,7.14353480416943,-0.459833057403451));
#9749=CARTESIAN_POINT('Ctrl Pts',(-0.0254605253309101,7.13594714126297,
-0.465066394981859));
#9750=CARTESIAN_POINT('Ctrl Pts',(-0.100983732313105,7.1689565884905,-0.470299732560268));
#9751=CARTESIAN_POINT('Ctrl Pts',(-0.176506939295298,7.20196603571802,-0.475533070138676));
#9752=CARTESIAN_POINT('Ctrl Pts',(-0.234286088180962,7.27557259307953,-0.480766407717085));
#9753=CARTESIAN_POINT('Ctrl Pts',(-0.248415620360814,7.35677440798752,-0.485999745295493));
#9754=CARTESIAN_POINT('Ctrl Pts',(-0.250883268666544,7.37095587687334,-0.48691372011393));
#9755=CARTESIAN_POINT('Ctrl Pts',(-0.252019569570078,7.38536900704663,-0.487827694932366));
#9756=CARTESIAN_POINT('Ctrl Pts',(-0.251895025789683,7.3998017247554,-0.488741669750802));
#9757=CARTESIAN_POINT('Ctrl Pts',(-0.251454189985941,7.399856210792,-0.461258330249197));
#9758=CARTESIAN_POINT('Ctrl Pts',(-0.251622064923045,7.36835465926041,-0.45927234327331));
#9759=CARTESIAN_POINT('Ctrl Pts',(-0.246123277962045,7.33690956728528,-0.457286356297422));
#9760=CARTESIAN_POINT('Ctrl Pts',(-0.234685894568262,7.30779760576974,-0.455300369321535));
#9761=CARTESIAN_POINT('Ctrl Pts',(-0.204546881050007,7.23108374811093,-0.450067031743127));
#9762=CARTESIAN_POINT('Ctrl Pts',(-0.133170729078467,7.17057096167843,-0.444833694164718));
#9763=CARTESIAN_POINT('Ctrl Pts',(-0.0525592787470221,7.15339044455997,
-0.43960035658631));
#9764=CARTESIAN_POINT('Ctrl Pts',(0.0280521715844237,7.13620992744151,-0.434367019007901));
#9765=CARTESIAN_POINT('Ctrl Pts',(0.117898920275772,7.1623616796371,-0.429133681429493));
#9766=CARTESIAN_POINT('Ctrl Pts',(0.176697746566812,7.22012043759096,-0.423900343851084));
#9767=CARTESIAN_POINT('Ctrl Pts',(0.23549657285785,7.27787919554482,-0.418667006272676));
#9768=CARTESIAN_POINT('Ctrl Pts',(0.26324747674858,7.36724495925696,-0.413433668694268));
#9769=CARTESIAN_POINT('Ctrl Pts',(0.247508207368464,7.44815015991153,-0.408200331115859));
#9770=CARTESIAN_POINT('Ctrl Pts',(0.231768937988348,7.52905536056611,-0.402966993537451));
#9771=CARTESIAN_POINT('Ctrl Pts',(0.172539495337386,7.60149999816312,-0.397733655959042));
#9772=CARTESIAN_POINT('Ctrl Pts',(0.0963756841381397,7.63300317191756,-0.392500318380633));
#9773=CARTESIAN_POINT('Ctrl Pts',(0.0202118729388946,7.664506345672,-0.387266980802225));
#9774=CARTESIAN_POINT('Ctrl Pts',(-0.0728863068086339,7.65506805558386,
-0.382033643223817));
#9775=CARTESIAN_POINT('Ctrl Pts',(-0.141177839644895,7.60892000431816,-0.376800305645409));
#9776=CARTESIAN_POINT('Ctrl Pts',(-0.208781945514779,7.56323648230766,-0.371619647180005));
#9777=CARTESIAN_POINT('Ctrl Pts',(-0.252076301533613,7.48157852511813,-0.366438988714601));
#9778=CARTESIAN_POINT('Ctrl Pts',(-0.252147107674537,7.3999852313674,-0.361258330249197));
#9779=CARTESIAN_POINT('Origin',(0.,7.4,-0.45));
#9780=CARTESIAN_POINT('',(-0.251485840701091,7.40016248328612,-0.261258330249198));
#9781=CARTESIAN_POINT('',(-0.251389294427012,7.3999184928281,-0.288741669750802));
#9782=CARTESIAN_POINT('',(-0.25175,7.4,-0.45));
#9783=CARTESIAN_POINT('Ctrl Pts',(-0.251389294427012,7.3999184928281,-0.288741669750802));
#9784=CARTESIAN_POINT('Ctrl Pts',(-0.251250073158243,7.44678343134187,-0.291694310658131));
#9785=CARTESIAN_POINT('Ctrl Pts',(-0.238659177002226,7.49371785771873,-0.29464695156546));
#9786=CARTESIAN_POINT('Ctrl Pts',(-0.214093468541586,7.53320194788991,-0.297599592472789));
#9787=CARTESIAN_POINT('Ctrl Pts',(-0.170552567611783,7.60318457677283,-0.302832930051198));
#9788=CARTESIAN_POINT('Ctrl Pts',(-0.0893928656252568,7.64976201913611,
-0.308066267629606));
#9789=CARTESIAN_POINT('Ctrl Pts',(-0.00700270411693429,7.65205105509271,
-0.313299605208015));
#9790=CARTESIAN_POINT('Ctrl Pts',(0.075387457391387,7.65434009104931,-0.318532942786423));
#9791=CARTESIAN_POINT('Ctrl Pts',(0.159008078421505,7.61234072059923,-0.323766280364831));
#9792=CARTESIAN_POINT('Ctrl Pts',(0.206367452347224,7.54488356303595,-0.32899961794324));
#9793=CARTESIAN_POINT('Ctrl Pts',(0.253726826272944,7.47742640547267,-0.334232955521648));
#9794=CARTESIAN_POINT('Ctrl Pts',(0.264824953094265,7.3845114607962,-0.339466293100057));
#9795=CARTESIAN_POINT('Ctrl Pts',(0.234685934453829,7.30779759009962,-0.344699630678465));
#9796=CARTESIAN_POINT('Ctrl Pts',(0.204546915813393,7.23108371940303,-0.349932968256874));
#9797=CARTESIAN_POINT('Ctrl Pts',(0.133170751711201,7.17057092268632,-0.355166305835282));
#9798=CARTESIAN_POINT('Ctrl Pts',(0.0525592876795934,7.15339040264801,-0.360399643413691));
#9799=CARTESIAN_POINT('Ctrl Pts',(-0.0280521763520133,7.13620988260969,
-0.365632980992099));
#9800=CARTESIAN_POINT('Ctrl Pts',(-0.117898940313035,7.16236163924978,-0.370866318570508));
#9801=CARTESIAN_POINT('Ctrl Pts',(-0.176697776597091,7.2201204070199,-0.376099656148916));
#9802=CARTESIAN_POINT('Ctrl Pts',(-0.2240439603623,7.26662910354725,-0.380313660682878));
#9803=CARTESIAN_POINT('Ctrl Pts',(-0.251259154956394,7.3336312901848,-0.38452766521684));
#9804=CARTESIAN_POINT('Ctrl Pts',(-0.251847334099258,7.40020792401048,-0.388741669750802));
#9805=CARTESIAN_POINT('Ctrl Pts',(-0.252147107674537,7.3999852313674,-0.361258330249197));
#9806=CARTESIAN_POINT('Ctrl Pts',(-0.252147827661142,7.39915555645819,-0.361205651136192));
#9807=CARTESIAN_POINT('Ctrl Pts',(-0.252144078472191,7.39832588823498,-0.361152972023188));
#9808=CARTESIAN_POINT('Ctrl Pts',(-0.252135840222057,7.3974962645886,-0.361100292910183));
#9809=CARTESIAN_POINT('Ctrl Pts',(-0.251317422037965,7.31507838856804,-0.355866955331774));
#9810=CARTESIAN_POINT('Ctrl Pts',(-0.206195699744786,7.2331004489702,-0.350633617753366));
#9811=CARTESIAN_POINT('Ctrl Pts',(-0.137001213984329,7.1883176483633,-0.345400280174958));
#9812=CARTESIAN_POINT('Ctrl Pts',(-0.0678067282238716,7.14353484775639,
-0.340166942596549));
#9813=CARTESIAN_POINT('Ctrl Pts',(0.0254605210038648,7.13594718614041,-0.334933605018141));
#9814=CARTESIAN_POINT('Ctrl Pts',(0.100983715150651,7.16895662775745,-0.329700267439732));
#9815=CARTESIAN_POINT('Ctrl Pts',(0.176506909297436,7.20196606937449,-0.324466929861324));
#9816=CARTESIAN_POINT('Ctrl Pts',(0.234286048363272,7.27557261422455,-0.319233592282915));
#9817=CARTESIAN_POINT('Ctrl Pts',(0.248415578141833,7.35677441533289,-0.314000254704507));
#9818=CARTESIAN_POINT('Ctrl Pts',(0.262545107920394,7.43797621644123,-0.308766917126099));
#9819=CARTESIAN_POINT('Ctrl Pts',(0.233025028411682,7.52677327380785,-0.30353357954769));
#9820=CARTESIAN_POINT('Ctrl Pts',(0.173090808970175,7.58335299984742,-0.298300241969282));
#9821=CARTESIAN_POINT('Ctrl Pts',(0.113156589528667,7.63993272588698,-0.293066904390873));
#9822=CARTESIAN_POINT('Ctrl Pts',(0.022808230154364,7.6642951205995,-0.287833566812465));
#9823=CARTESIAN_POINT('Ctrl Pts',(-0.0574461490583136,7.64551718942048,
-0.282600229234056));
#9824=CARTESIAN_POINT('Ctrl Pts',(-0.137700528270991,7.62673925824146,-0.277366891655648));
#9825=CARTESIAN_POINT('Ctrl Pts',(-0.207860927322042,7.56482100117091,-0.272133554077239));
#9826=CARTESIAN_POINT('Ctrl Pts',(-0.236470594324117,7.48752376180974,-0.266900216498831));
#9827=CARTESIAN_POINT('Ctrl Pts',(-0.246751636103367,7.45974657211945,-0.265019587748953));
#9828=CARTESIAN_POINT('Ctrl Pts',(-0.251666966336733,7.4299833961716,-0.263138958999075));
#9829=CARTESIAN_POINT('Ctrl Pts',(-0.251485840701091,7.40016248328612,-0.261258330249198));
#9830=CARTESIAN_POINT('Origin',(0.,7.4,-0.45));
#9831=CARTESIAN_POINT('',(-0.251664502419995,7.39978648873079,-0.161258330249198));
#9832=CARTESIAN_POINT('',(-0.252102618136395,7.39990630057405,-0.188741669750802));
#9833=CARTESIAN_POINT('',(-0.25175,7.4,-0.45));
#9834=CARTESIAN_POINT('Ctrl Pts',(-0.252102618136395,7.39990630057405,-0.188741669750802));
#9835=CARTESIAN_POINT('Ctrl Pts',(-0.251729671980332,7.47689446754405,-0.193627618521014));
#9836=CARTESIAN_POINT('Ctrl Pts',(-0.213827741655731,7.55420081887498,-0.198513567291225));
#9837=CARTESIAN_POINT('Ctrl Pts',(-0.152559928540191,7.60075915469979,-0.203399516061437));
#9838=CARTESIAN_POINT('Ctrl Pts',(-0.0869360008643037,7.65062776772039,
-0.208632853639846));
#9839=CARTESIAN_POINT('Ctrl Pts',(0.00549453556043952,7.66522058873043,
-0.213866191218254));
#9840=CARTESIAN_POINT('Ctrl Pts',(0.0832900168929199,7.63799484419977,-0.219099528796662));
#9841=CARTESIAN_POINT('Ctrl Pts',(0.1610854982254,7.61076909966911,-0.224332866375071));
#9842=CARTESIAN_POINT('Ctrl Pts',(0.224245924465617,7.54172478959775,-0.229566203953479));
#9843=CARTESIAN_POINT('Ctrl Pts',(0.24445301032052,7.46181826765958,-0.234799541531888));
#9844=CARTESIAN_POINT('Ctrl Pts',(0.264660096175424,7.38191174572141,-0.240032879110296));
#9845=CARTESIAN_POINT('Ctrl Pts',(0.241913841645014,7.29114301191644,-0.245266216688705));
#9846=CARTESIAN_POINT('Ctrl Pts',(0.186412641644911,7.23020866043887,-0.250499554267113));
#9847=CARTESIAN_POINT('Ctrl Pts',(0.13091144164481,7.16927430896129,-0.255732891845522));
#9848=CARTESIAN_POINT('Ctrl Pts',(0.042655296175016,7.13817433981112,-0.26096622942393));
#9849=CARTESIAN_POINT('Ctrl Pts',(-0.0387857298803423,7.1508525748262,-0.266199567002338));
#9850=CARTESIAN_POINT('Ctrl Pts',(-0.120226755935702,7.16353080984128,-0.271432904580747));
#9851=CARTESIAN_POINT('Ctrl Pts',(-0.194852662576626,7.2199872490216,-0.276666242159155));
#9852=CARTESIAN_POINT('Ctrl Pts',(-0.229204565960548,7.29490937631304,-0.281899579737564));
#9853=CARTESIAN_POINT('Ctrl Pts',(-0.24417517898123,7.32756055612776,-0.284180276408643));
#9854=CARTESIAN_POINT('Ctrl Pts',(-0.251496832557856,7.36371879479052,-0.286460973079723));
#9855=CARTESIAN_POINT('Ctrl Pts',(-0.251389294427012,7.3999184928281,-0.288741669750802));
#9856=CARTESIAN_POINT('Ctrl Pts',(-0.251485840701091,7.40016248328612,-0.261258330249198));
#9857=CARTESIAN_POINT('Ctrl Pts',(-0.251162937247801,7.34699896660984,-0.257905621420667));
#9858=CARTESIAN_POINT('Ctrl Pts',(-0.234642316978043,7.293651948577,-0.254552912592136));
#9859=CARTESIAN_POINT('Ctrl Pts',(-0.203449588637141,7.2510469333767,-0.251200203763606));
#9860=CARTESIAN_POINT('Ctrl Pts',(-0.154759980994992,7.18454356595661,-0.245966866185197));
#9861=CARTESIAN_POINT('Ctrl Pts',(-0.0703218307575955,7.14421305276819,
-0.240733528606789));
#9862=CARTESIAN_POINT('Ctrl Pts',(0.0120066141281704,7.14813775672736,-0.23550019102838));
#9863=CARTESIAN_POINT('Ctrl Pts',(0.0943350590139364,7.15206246068653,-0.230266853449972));
#9864=CARTESIAN_POINT('Ctrl Pts',(0.174553798548072,7.2002423817933,-0.225033515871563));
#9865=CARTESIAN_POINT('Ctrl Pts',(0.216696372552131,7.27107585384036,-0.219800178293155));
#9866=CARTESIAN_POINT('Ctrl Pts',(0.258838946556191,7.34190932588742,-0.214566840714746));
#9867=CARTESIAN_POINT('Ctrl Pts',(0.262905355030174,7.43539634887478,-0.209333503136338));
#9868=CARTESIAN_POINT('Ctrl Pts',(0.227072411321265,7.50962150200167,-0.204100165557929));
#9869=CARTESIAN_POINT('Ctrl Pts',(0.191239467612356,7.58384665512856,-0.198866827979521));
#9870=CARTESIAN_POINT('Ctrl Pts',(0.115507171720556,7.63880993839499,-0.193633490401113));
#9871=CARTESIAN_POINT('Ctrl Pts',(0.0338304474764224,7.64986843242236,-0.188400152822704));
#9872=CARTESIAN_POINT('Ctrl Pts',(-0.0478462767677109,7.66092692644973,
-0.183166815244296));
#9873=CARTESIAN_POINT('Ctrl Pts',(-0.135467429364177,7.62808063123805,-0.177933477665887));
#9874=CARTESIAN_POINT('Ctrl Pts',(-0.189747617397774,7.56605607392972,-0.172700140087479));
#9875=CARTESIAN_POINT('Ctrl Pts',(-0.229305775721628,7.5208539965815,-0.168886203474718));
#9876=CARTESIAN_POINT('Ctrl Pts',(-0.251156011991034,7.4601548753515,-0.165072266861958));
#9877=CARTESIAN_POINT('Ctrl Pts',(-0.251664502419995,7.39978648873079,-0.161258330249198));
#9878=CARTESIAN_POINT('Origin',(0.,7.4,-0.45));
#9879=CARTESIAN_POINT('',(-0.252053546614158,7.40012638988493,-0.0612583302491975));
#9880=CARTESIAN_POINT('',(-0.25159361924534,7.40020120251426,-0.088741669750802));
#9881=CARTESIAN_POINT('',(-0.25175,7.4,-0.45));
#9882=CARTESIAN_POINT('',(0.191346599666508,7.56359872033749,0.));
#9883=CARTESIAN_POINT('Ctrl Pts',(-0.252053546614158,7.40012638988493,-0.0612583302491975));
#9884=CARTESIAN_POINT('Ctrl Pts',(-0.251574518405349,7.32573800995496,-0.0565388995680237));
#9885=CARTESIAN_POINT('Ctrl Pts',(-0.216528551878887,7.25097281135749,-0.0518194688868499));
#9886=CARTESIAN_POINT('Ctrl Pts',(-0.158787371836513,7.20414745955911,-0.047100038205676));
#9887=CARTESIAN_POINT('Ctrl Pts',(-0.0947586557155584,7.15222321493229,
-0.0418667006272676));
#9888=CARTESIAN_POINT('Ctrl Pts',(-0.00282297831979787,7.13465494682447,
-0.0366333630488591));
#9889=CARTESIAN_POINT('Ctrl Pts',(0.0757847255684538,7.15946950281323,-0.0314000254704506));
#9890=CARTESIAN_POINT('Ctrl Pts',(0.154392429456705,7.18428405880198,-0.0261666878920422));
#9891=CARTESIAN_POINT('Ctrl Pts',(0.219672159837449,7.25148143888729,-0.0209333503136337));
#9892=CARTESIAN_POINT('Ctrl Pts',(0.242359347375236,7.33058044279975,-0.0157000127352253));
#9893=CARTESIAN_POINT('Ctrl Pts',(0.265046534913023,7.40967944671221,-0.0104666751568168));
#9894=CARTESIAN_POINT('Ctrl Pts',(0.245141179607854,7.50068007445182,-0.00523333757840841));
#9895=CARTESIAN_POINT('Ctrl Pts',(0.191346599666508,7.56359872033749,2.72395540626932E-17));
#9896=CARTESIAN_POINT('',(-0.191702394569677,7.56382704462399,5.75771190526024E-16));
#9897=CARTESIAN_POINT('Origin',(0.,7.4,0.));
#9898=CARTESIAN_POINT('Ctrl Pts',(-0.191704062602126,7.56382811505056,3.81639164714898E-16));
#9899=CARTESIAN_POINT('Ctrl Pts',(-0.140332590985575,7.6235382994157,-0.00499978774624405));
#9900=CARTESIAN_POINT('Ctrl Pts',(-0.0585928881206123,7.65757754738541,
-0.00999957549248847));
#9901=CARTESIAN_POINT('Ctrl Pts',(0.0199179745523958,7.65134629866448,-0.0149993632387329));
#9902=CARTESIAN_POINT('Ctrl Pts',(0.102096232669162,7.64482397616866,-0.0202327008171413));
#9903=CARTESIAN_POINT('Ctrl Pts',(0.180736954405333,7.59418105970145,-0.0254660383955498));
#9904=CARTESIAN_POINT('Ctrl Pts',(0.220629145239623,7.52206769251925,-0.0306993759739582));
#9905=CARTESIAN_POINT('Ctrl Pts',(0.260521336073913,7.44995432533705,-0.0359327135523667));
#9906=CARTESIAN_POINT('Ctrl Pts',(0.261664996006322,7.35637050743987,-0.0411660511307752));
#9907=CARTESIAN_POINT('Ctrl Pts',(0.22352361367014,7.28330257532835,-0.0463993887091836));
#9908=CARTESIAN_POINT('Ctrl Pts',(0.185382231333959,7.21023464321682,-0.0516327262875921));
#9909=CARTESIAN_POINT('Ctrl Pts',(0.107955806729186,7.15768259689094,-0.0568660638660005));
#9910=CARTESIAN_POINT('Ctrl Pts',(0.0259706171598658,7.14919473271428,-0.0620994014444089));
#9911=CARTESIAN_POINT('Ctrl Pts',(-0.0560145724094547,7.14070686853762,
-0.0673327390228173));
#9912=CARTESIAN_POINT('Ctrl Pts',(-0.142558526943323,7.17628318651017,-0.0725660766012259));
#9913=CARTESIAN_POINT('Ctrl Pts',(-0.19486468239543,7.239979646976,-0.0777994141796343));
#9914=CARTESIAN_POINT('Ctrl Pts',(-0.231319896193954,7.28437342939836,-0.0814468327033569));
#9915=CARTESIAN_POINT('Ctrl Pts',(-0.251144065024393,7.34242659901433,-0.0850942512270795));
#9916=CARTESIAN_POINT('Ctrl Pts',(-0.25159361924534,7.40020120251426,-0.088741669750802));
#9917=CARTESIAN_POINT('Origin',(7.4,0.,-0.45));
#9918=CARTESIAN_POINT('',(7.14864152176833,-9.8905947593236E-6,-0.761258330249198));
#9919=CARTESIAN_POINT('',(7.1484153974468,-0.000333656346126327,-0.788741669750802));
#9920=CARTESIAN_POINT('',(7.14825,3.08304831685346E-17,-0.45));
#9921=CARTESIAN_POINT('',(7.20865340033349,0.163598720337494,-0.8));
#9922=CARTESIAN_POINT('Ctrl Pts',(7.1484153974468,-0.000333656346126327,
-0.788741669750802));
#9923=CARTESIAN_POINT('Ctrl Pts',(7.14892873762876,0.0589216799335651,-0.792494446500535));
#9924=CARTESIAN_POINT('Ctrl Pts',(7.1700778171916,0.118480356030442,-0.796247223250267));
#9925=CARTESIAN_POINT('Ctrl Pts',(7.2086534003335,0.163598720337496,-0.8));
#9926=CARTESIAN_POINT('',(7.59170237435269,0.16382705780558,-0.8));
#9927=CARTESIAN_POINT('Origin',(7.4,0.,-0.8));
#9928=CARTESIAN_POINT('Ctrl Pts',(7.59170404101736,0.163828127476929,-0.8));
#9929=CARTESIAN_POINT('Ctrl Pts',(7.54033256376596,0.223538338460724,-0.795000212253756));
#9930=CARTESIAN_POINT('Ctrl Pts',(7.45859287630538,0.257577514423726,-0.790000424507512));
#9931=CARTESIAN_POINT('Ctrl Pts',(7.38008202560527,0.251346250864262,-0.785000636761268));
#9932=CARTESIAN_POINT('Ctrl Pts',(7.29790378002067,0.244823912836771,-0.779767299182859));
#9933=CARTESIAN_POINT('Ctrl Pts',(7.21926306705711,0.19418104347167,-0.77453396160445));
#9934=CARTESIAN_POINT('Ctrl Pts',(7.17937087924982,0.122067692789386,-0.769300624026042));
#9935=CARTESIAN_POINT('Ctrl Pts',(7.15893620195638,0.0851278022809988,-0.766619859433761));
#9936=CARTESIAN_POINT('Ctrl Pts',(7.14866904464232,0.0425541090180851,-0.763939094841479));
#9937=CARTESIAN_POINT('Ctrl Pts',(7.14864152176833,-9.8905947593236E-6,
-0.761258330249198));
#9938=CARTESIAN_POINT('Origin',(7.4,0.,-0.45));
#9939=CARTESIAN_POINT('',(7.14798283450166,-0.000154017160047509,-0.661258330249198));
#9940=CARTESIAN_POINT('',(7.14792656787638,0.000120390219947525,-0.688741669750802));
#9941=CARTESIAN_POINT('',(7.14825,3.08304831685346E-17,-0.45));
#9942=CARTESIAN_POINT('Ctrl Pts',(7.14792656787638,0.000120390219947525,
-0.688741669750802));
#9943=CARTESIAN_POINT('Ctrl Pts',(7.14788433994059,0.00725647209880052,
-0.689194416785009));
#9944=CARTESIAN_POINT('Ctrl Pts',(7.14816172440802,0.014389202158696,-0.689647163819216));
#9945=CARTESIAN_POINT('Ctrl Pts',(7.14876949662151,0.0214936402017243,-0.690099910853423));
#9946=CARTESIAN_POINT('Ctrl Pts',(7.15579478209814,0.103614382636149,-0.695333248431831));
#9947=CARTESIAN_POINT('Ctrl Pts',(7.20696391712096,0.18195496508943,-0.70056658601024));
#9948=CARTESIAN_POINT('Ctrl Pts',(7.27933593931993,0.221399912316197,-0.705799923588648));
#9949=CARTESIAN_POINT('Ctrl Pts',(7.3517079615189,0.260844859542965,-0.711033261167056));
#9950=CARTESIAN_POINT('Ctrl Pts',(7.44528287089401,0.261394171543217,-0.716266598745465));
#9951=CARTESIAN_POINT('Ctrl Pts',(7.51810396235645,0.222783607866771,-0.721499936323873));
#9952=CARTESIAN_POINT('Ctrl Pts',(7.5909250538189,0.184173044190324,-0.726733273902282));
#9953=CARTESIAN_POINT('Ctrl Pts',(7.64299232736868,0.10640260483718,-0.73196661148069));
#9954=CARTESIAN_POINT('Ctrl Pts',(7.65096509106803,0.0243772648179821,-0.737199949059099));
#9955=CARTESIAN_POINT('Ctrl Pts',(7.65893785476737,-0.0576480752012157,
-0.742433286637507));
#9956=CARTESIAN_POINT('Ctrl Pts',(7.62281610861627,-0.143928315886467,-0.747666624215916));
#9957=CARTESIAN_POINT('Ctrl Pts',(7.55878738396318,-0.195852557959908,-0.752899961794324));
#9958=CARTESIAN_POINT('Ctrl Pts',(7.4947586593101,-0.247776800033349,-0.758133299372733));
#9959=CARTESIAN_POINT('Ctrl Pts',(7.40282295615504,-0.26534504349498,-0.763366636951141));
#9960=CARTESIAN_POINT('Ctrl Pts',(7.32421526476616,-0.240530499385705,-0.768599974529549));
#9961=CARTESIAN_POINT('Ctrl Pts',(7.24560757337728,-0.215715955276429,-0.773833312107958));
#9962=CARTESIAN_POINT('Ctrl Pts',(7.18032789375458,-0.148518623596246,-0.779066649686366));
#9963=CARTESIAN_POINT('Ctrl Pts',(7.1576407055083,-0.0694196161641834,-0.784299987264775));
#9964=CARTESIAN_POINT('Ctrl Pts',(7.1512222848108,-0.0470417568657088,-0.785780548093451));
#9965=CARTESIAN_POINT('Ctrl Pts',(7.14821287237913,-0.0237113139144776,
-0.787261108922126));
#9966=CARTESIAN_POINT('Ctrl Pts',(7.1484153974468,-0.000333656346126327,
-0.788741669750802));
#9967=CARTESIAN_POINT('Ctrl Pts',(7.14864152176833,-9.8905947593236E-6,
-0.761258330249198));
#9968=CARTESIAN_POINT('Ctrl Pts',(7.14861531501193,-0.0405385203394587,
-0.758705757263071));
#9969=CARTESIAN_POINT('Ctrl Pts',(7.15787285816352,-0.0810583613501985,
-0.756153184276944));
#9970=CARTESIAN_POINT('Ctrl Pts',(7.17647640716818,-0.116697419870879,-0.753600611290817));
#9971=CARTESIAN_POINT('Ctrl Pts',(7.21461778554483,-0.189765349849391,-0.748367273712409));
#9972=CARTESIAN_POINT('Ctrl Pts',(7.29204420494912,-0.242317377806947,-0.743133936134));
#9973=CARTESIAN_POINT('Ctrl Pts',(7.37402938660657,-0.250805238180063,-0.737900598555592));
#9974=CARTESIAN_POINT('Ctrl Pts',(7.45601456826403,-0.25929309855318,-0.732667260977183));
#9975=CARTESIAN_POINT('Ctrl Pts',(7.54255851217464,-0.223716791341859,-0.727433923398775));
#9976=CARTESIAN_POINT('Ctrl Pts',(7.59486466202115,-0.160020338937948,-0.722200585820367));
#9977=CARTESIAN_POINT('Ctrl Pts',(7.64717081186766,-0.096323886534038,-0.716967248241958));
#9978=CARTESIAN_POINT('Ctrl Pts',(7.66523916765007,-0.00450728893753763,
-0.71173391066355));
#9979=CARTESIAN_POINT('Ctrl Pts',(7.6409658021157,0.0742596779135476,-0.706500573085141));
#9980=CARTESIAN_POINT('Ctrl Pts',(7.61669243658134,0.153026644764634,-0.701267235506733));
#9981=CARTESIAN_POINT('Ctrl Pts',(7.55007734973019,0.218743980870306,-0.696033897928324));
#9982=CARTESIAN_POINT('Ctrl Pts',(7.47098916964924,0.241948671073236,-0.690800560349916));
#9983=CARTESIAN_POINT('Ctrl Pts',(7.39190098956829,0.265153361276165,-0.685567222771507));
#9984=CARTESIAN_POINT('Ctrl Pts',(7.30033971625753,0.245845405576353,-0.680333885193099));
#9985=CARTESIAN_POINT('Ctrl Pts',(7.23735657471084,0.192680791744281,-0.675100547614691));
#9986=CARTESIAN_POINT('Ctrl Pts',(7.18182627990447,0.145807190223893,-0.670486475159527));
#9987=CARTESIAN_POINT('Ctrl Pts',(7.14851092559648,0.0726154356453729,-0.665872402704362));
#9988=CARTESIAN_POINT('Ctrl Pts',(7.14798283450166,-0.000154017160047509,
-0.661258330249198));
#9989=CARTESIAN_POINT('Origin',(7.4,0.,-0.45));
#9990=CARTESIAN_POINT('',(7.14828831497717,0.000216666477491244,-0.561258330249198));
#9991=CARTESIAN_POINT('',(7.14862473855677,5.66816876182724E-5,-0.588741669750802));
#9992=CARTESIAN_POINT('',(7.14825,3.08304831685346E-17,-0.45));
#9993=CARTESIAN_POINT('Ctrl Pts',(7.14862473855677,5.66816876182724E-5,
-0.588741669750802));
#9994=CARTESIAN_POINT('Ctrl Pts',(7.14854678397043,0.0379339368751698,-0.591127724647892));
#9995=CARTESIAN_POINT('Ctrl Pts',(7.1565901316137,0.0757797576445921,-0.593513779544981));
#9996=CARTESIAN_POINT('Ctrl Pts',(7.17292757848469,0.109621506901428,-0.595899834442071));
#9997=CARTESIAN_POINT('Ctrl Pts',(7.20876052379935,0.183846663380813,-0.601133172020479));
#9998=CARTESIAN_POINT('Ctrl Pts',(7.28449282307928,0.238809949198099,-0.606366509598887));
#9999=CARTESIAN_POINT('Ctrl Pts',(7.3661695509983,0.249868443686133,-0.611599847177296));
#10000=CARTESIAN_POINT('Ctrl Pts',(7.44784627891733,0.260926938174167,-0.616833184755704));
#10001=CARTESIAN_POINT('Ctrl Pts',(7.53546743547544,0.228080641332948,-0.622066522334113));
#10002=CARTESIAN_POINT('Ctrl Pts',(7.58974762593152,0.166056081305598,-0.627299859912522));
#10003=CARTESIAN_POINT('Ctrl Pts',(7.64402781638759,0.104031521278249,-0.63253319749093));
#10004=CARTESIAN_POINT('Ctrl Pts',(7.66496704074163,0.0128286980647704,
-0.637766535069338));
#10005=CARTESIAN_POINT('Ctrl Pts',(7.64317715560285,-0.0666606273237503,
-0.642999872647746));
#10006=CARTESIAN_POINT('Ctrl Pts',(7.62138727046407,-0.146149952712272,
-0.648233210226155));
#10007=CARTESIAN_POINT('Ctrl Pts',(7.55686827583247,-0.213925780275835,
-0.653466547804564));
#10008=CARTESIAN_POINT('Ctrl Pts',(7.47854745486387,-0.23960157726169,-0.658699885382972));
#10009=CARTESIAN_POINT('Ctrl Pts',(7.40022663389526,-0.265277374247545,
-0.663933222961381));
#10010=CARTESIAN_POINT('Ctrl Pts',(7.30810398658965,-0.248853140655693,
-0.669166560539789));
#10011=CARTESIAN_POINT('Ctrl Pts',(7.24348338090206,-0.197690572651982,
-0.674399898118197));
#10012=CARTESIAN_POINT('Ctrl Pts',(7.18445323964283,-0.150954185948262,
-0.679180488662399));
#10013=CARTESIAN_POINT('Ctrl Pts',(7.14837245587845,-0.0752300438529192,
-0.683961079206601));
#10014=CARTESIAN_POINT('Ctrl Pts',(7.14792656787638,0.000120390219947525,
-0.688741669750802));
#10015=CARTESIAN_POINT('Ctrl Pts',(7.14798283450166,-0.000154017160047509,
-0.661258330249198));
#10016=CARTESIAN_POINT('Ctrl Pts',(7.14791195819876,-0.00992057037260971,
-0.660639065125954));
#10017=CARTESIAN_POINT('Ctrl Pts',(7.14843167665666,-0.0196795166918168,
-0.660019800002709));
#10018=CARTESIAN_POINT('Ctrl Pts',(7.14956754906296,-0.0293662095570414,
-0.659400534879465));
#10019=CARTESIAN_POINT('Ctrl Pts',(7.15916667474439,-0.111227325061965,
-0.654167197301056));
#10020=CARTESIAN_POINT('Ctrl Pts',(7.21276993588987,-0.187928284107481,
-0.648933859722648));
#10021=CARTESIAN_POINT('Ctrl Pts',(7.28634387847187,-0.225080046990995,
-0.643700522144239));
#10022=CARTESIAN_POINT('Ctrl Pts',(7.35991782105388,-0.262231809874509,
-0.638467184565831));
#10023=CARTESIAN_POINT('Ctrl Pts',(7.45346244507241,-0.259834376596021,
-0.633233846987423));
#10024=CARTESIAN_POINT('Ctrl Pts',(7.52503665627896,-0.218962547126307,
-0.628000509409014));
#10025=CARTESIAN_POINT('Ctrl Pts',(7.59661086748551,-0.178090717656593,
-0.622767171830606));
#10026=CARTESIAN_POINT('Ctrl Pts',(7.64621466588009,-0.0987444919956527,
-0.617533834252197));
#10027=CARTESIAN_POINT('Ctrl Pts',(7.65160790755967,-0.0164991809676121,
-0.612300496673789));
#10028=CARTESIAN_POINT('Ctrl Pts',(7.65700114923926,0.0657461300604286,
-0.60706715909538));
#10029=CARTESIAN_POINT('Ctrl Pts',(7.61818383420385,0.15089052645557,-0.601833821516972));
#10030=CARTESIAN_POINT('Ctrl Pts',(7.55255991314267,0.20075913443422,-0.596600483938564));
#10031=CARTESIAN_POINT('Ctrl Pts',(7.48693599208148,0.25062774241287,-0.591367146360156));
#10032=CARTESIAN_POINT('Ctrl Pts',(7.39450546499451,0.26522056197503,-0.586133808781746));
#10033=CARTESIAN_POINT('Ctrl Pts',(7.31670999151327,0.23799482019678,-0.580900471203338));
#10034=CARTESIAN_POINT('Ctrl Pts',(7.23891451803204,0.21076907841853,-0.575667133624929));
#10035=CARTESIAN_POINT('Ctrl Pts',(7.17575409815654,0.14172477529987,-0.570433796046521));
#10036=CARTESIAN_POINT('Ctrl Pts',(7.15554701433853,0.0618182614198286,
-0.565200458468113));
#10037=CARTESIAN_POINT('Ctrl Pts',(7.15047320219045,0.0417544736666595,
-0.563886415728475));
#10038=CARTESIAN_POINT('Ctrl Pts',(7.14810745066301,0.0210058607540061,
-0.562572372988836));
#10039=CARTESIAN_POINT('Ctrl Pts',(7.14828831497717,0.000216666477491244,
-0.561258330249198));
#10040=CARTESIAN_POINT('Origin',(7.4,0.,-0.45));
#10041=CARTESIAN_POINT('',(7.14854579264603,-0.000143789217906781,-0.461258330249198));
#10042=CARTESIAN_POINT('',(7.14810500570899,-0.000198275220022497,-0.488741669750802));
#10043=CARTESIAN_POINT('',(7.14825,3.08304831685346E-17,-0.45));
#10044=CARTESIAN_POINT('Ctrl Pts',(7.14810500570899,-0.000198275220022497,
-0.488741669750802));
#10045=CARTESIAN_POINT('Ctrl Pts',(7.14869358833605,0.0680094416058214,
-0.493061032510774));
#10046=CARTESIAN_POINT('Ctrl Pts',(7.17744215705244,0.13665463081379,-0.497380395270747));
#10047=CARTESIAN_POINT('Ctrl Pts',(7.22690918325704,0.183353008080594,-0.501699758030719));
#10048=CARTESIAN_POINT('Ctrl Pts',(7.28684340538992,0.239932736661351,-0.506933095609127));
#10049=CARTESIAN_POINT('Ctrl Pts',(7.37719176882127,0.264295132469651,-0.512166433187535));
#10050=CARTESIAN_POINT('Ctrl Pts',(7.45744615163793,0.245517200446581,-0.517399770765944));
#10051=CARTESIAN_POINT('Ctrl Pts',(7.53770053445458,0.226739268423512,-0.522633108344352));
#10052=CARTESIAN_POINT('Ctrl Pts',(7.60786093665655,0.164821008569074,-0.527866445922761));
#10053=CARTESIAN_POINT('Ctrl Pts',(7.6364706049432,0.0875237657383382,-0.533099783501169));
#10054=CARTESIAN_POINT('Ctrl Pts',(7.66508027322986,0.0102265229076026,
-0.538333121079578));
#10055=CARTESIAN_POINT('Ctrl Pts',(7.65213920760121,-0.0824497028994303,
-0.543566458657986));
#10056=CARTESIAN_POINT('Ctrl Pts',(7.60344959777296,-0.148953073308844,
-0.548799796236394));
#10057=CARTESIAN_POINT('Ctrl Pts',(7.5547599879447,-0.215456443718259,-0.554033133814803));
#10058=CARTESIAN_POINT('Ctrl Pts',(7.47032183391684,-0.255786958730054,
-0.559266471393212));
#10059=CARTESIAN_POINT('Ctrl Pts',(7.38799338533328,-0.251862254589131,
-0.56449980897162));
#10060=CARTESIAN_POINT('Ctrl Pts',(7.30566493674973,-0.247937550448207,
-0.569733146550029));
#10061=CARTESIAN_POINT('Ctrl Pts',(7.22544619361049,-0.199757627154565,
-0.574966484128437));
#10062=CARTESIAN_POINT('Ctrl Pts',(7.18330361771556,-0.128924151937003,
-0.580199821706845));
#10063=CARTESIAN_POINT('Ctrl Pts',(7.16037526182527,-0.0903860442336708,
-0.583047104388164));
#10064=CARTESIAN_POINT('Ctrl Pts',(7.14871776187482,-0.0451423004661291,
-0.585894387069483));
#10065=CARTESIAN_POINT('Ctrl Pts',(7.14862473855677,5.66816876182724E-5,
-0.588741669750802));
#10066=CARTESIAN_POINT('Ctrl Pts',(7.14828831497717,0.000216666477491244,
-0.561258330249198));
#10067=CARTESIAN_POINT('Ctrl Pts',(7.14882776514237,-0.0617896742390719,
-0.557339035410428));
#10068=CARTESIAN_POINT('Ctrl Pts',(7.17202202015866,-0.124157028526609,
-0.553419740571658));
#10069=CARTESIAN_POINT('Ctrl Pts',(7.21358737716188,-0.16979132243042,-0.549500445732887));
#10070=CARTESIAN_POINT('Ctrl Pts',(7.26908857156377,-0.230725667759206,
-0.544267108154479));
#10071=CARTESIAN_POINT('Ctrl Pts',(7.35734470812808,-0.261825633775355,
-0.539033770576071));
#10072=CARTESIAN_POINT('Ctrl Pts',(7.438785725967,-0.249147400040112,-0.533800432997662));
#10073=CARTESIAN_POINT('Ctrl Pts',(7.52022674380592,-0.236469166304868,
-0.528567095419254));
#10074=CARTESIAN_POINT('Ctrl Pts',(7.59485264291945,-0.180012732818235,
-0.523333757840845));
#10075=CARTESIAN_POINT('Ctrl Pts',(7.62920454283812,-0.105090613084703,
-0.518100420262437));
#10076=CARTESIAN_POINT('Ctrl Pts',(7.66355644275679,-0.0301684933511692,
-0.512867082684028));
#10077=CARTESIAN_POINT('Ctrl Pts',(7.65763434348059,0.0632193126292629,
-0.50763374510562));
#10078=CARTESIAN_POINT('Ctrl Pts',(7.61409344694317,0.133201934451936,-0.502400407527211));
#10079=CARTESIAN_POINT('Ctrl Pts',(7.57055255040575,0.203184556274608,-0.497167069948803));
#10080=CARTESIAN_POINT('Ctrl Pts',(7.4893928566071,0.249761993939521,-0.491933732370395));
#10081=CARTESIAN_POINT('Ctrl Pts',(7.40700270341056,0.252051029665313,-0.486700394791986));
#10082=CARTESIAN_POINT('Ctrl Pts',(7.32461255021403,0.254340065391105,-0.481467057213578));
#10083=CARTESIAN_POINT('Ctrl Pts',(7.24099193761961,0.212340699177775,-0.476233719635169));
#10084=CARTESIAN_POINT('Ctrl Pts',(7.19363256847158,0.144883548419682,-0.471000382056761));
#10085=CARTESIAN_POINT('Ctrl Pts',(7.16424549499626,0.103025553234657,-0.46775303145424));
#10086=CARTESIAN_POINT('Ctrl Pts',(7.14882029032525,0.0513654052804403,
-0.464505680851719));
#10087=CARTESIAN_POINT('Ctrl Pts',(7.14854579264603,-0.000143789217906781,
-0.461258330249198));
#10088=CARTESIAN_POINT('Origin',(7.4,0.,-0.45));
#10089=CARTESIAN_POINT('',(7.14785287490956,-1.4768633667023E-5,-0.361258330249198));
#10090=CARTESIAN_POINT('',(7.14815269739345,0.000207923984461611,-0.388741669750802));
#10091=CARTESIAN_POINT('',(7.14825,3.08304831685346E-17,-0.45));
#10092=CARTESIAN_POINT('Ctrl Pts',(7.14815269739345,0.000207923984461611,
-0.388741669750802));
#10093=CARTESIAN_POINT('Ctrl Pts',(7.14801042171326,0.0163122622245923,
-0.389761002795248));
#10094=CARTESIAN_POINT('Ctrl Pts',(7.14942613596003,0.032391700678434,-0.390780335839695));
#10095=CARTESIAN_POINT('Ctrl Pts',(7.15249178151693,0.0481501620737753,
-0.391799668884141));
#10096=CARTESIAN_POINT('Ctrl Pts',(7.16823105160384,0.129055366361475,-0.39703300646255));
#10097=CARTESIAN_POINT('Ctrl Pts',(7.22746049691456,0.201500007211662,-0.402266344040958));
#10098=CARTESIAN_POINT('Ctrl Pts',(7.30362431153402,0.233003182380788,-0.407499681619367));
#10099=CARTESIAN_POINT('Ctrl Pts',(7.37978812615348,0.264506357549914,-0.412733019197775));
#10100=CARTESIAN_POINT('Ctrl Pts',(7.47288631008167,0.255068067037979,-0.417966356776183));
#10101=CARTESIAN_POINT('Ctrl Pts',(7.54117784598463,0.20892001369993,-0.423199694354592));
#10102=CARTESIAN_POINT('Ctrl Pts',(7.60946938188759,0.162771960361881,-0.428433031933));
#10103=CARTESIAN_POINT('Ctrl Pts',(7.65295426976532,0.0799141441977179,
-0.433666369511409));
#10104=CARTESIAN_POINT('Ctrl Pts',(7.65213585154447,-0.00250373552386811,
-0.438899707089817));
#10105=CARTESIAN_POINT('Ctrl Pts',(7.65131743332362,-0.0849216152454548,
-0.444133044668226));
#10106=CARTESIAN_POINT('Ctrl Pts',(7.6061957090042,-0.166899558524465,-0.449366382246634));
#10107=CARTESIAN_POINT('Ctrl Pts',(7.5370012201365,-0.211682361142448,-0.454599719825042));
#10108=CARTESIAN_POINT('Ctrl Pts',(7.46780673126879,-0.25646516376043,-0.459833057403451));
#10109=CARTESIAN_POINT('Ctrl Pts',(7.37453947785282,-0.264052825717385,
-0.46506639498186));
#10110=CARTESIAN_POINT('Ctrl Pts',(7.29901628031458,-0.231043382617906,
-0.470299732560268));
#10111=CARTESIAN_POINT('Ctrl Pts',(7.22349308277634,-0.198033939518426,
-0.475533070138677));
#10112=CARTESIAN_POINT('Ctrl Pts',(7.16571394111585,-0.12442739136251,-0.480766407717085));
#10113=CARTESIAN_POINT('Ctrl Pts',(7.15158441070281,-0.0432255866079445,
-0.485999745295493));
#10114=CARTESIAN_POINT('Ctrl Pts',(7.14911676270564,-0.029044119495361,
-0.486913720113929));
#10115=CARTESIAN_POINT('Ctrl Pts',(7.14798046194419,-0.0146309911242199,
-0.487827694932365));
#10116=CARTESIAN_POINT('Ctrl Pts',(7.14810500570899,-0.000198275220022497,
-0.488741669750802));
#10117=CARTESIAN_POINT('Ctrl Pts',(7.14854579264603,-0.000143789217906781,
-0.461258330249198));
#10118=CARTESIAN_POINT('Ctrl Pts',(7.14837791769732,-0.03164534292534,-0.459272343273311));
#10119=CARTESIAN_POINT('Ctrl Pts',(7.15387670503811,-0.0630904370724168,
-0.457286356297423));
#10120=CARTESIAN_POINT('Ctrl Pts',(7.16531408922188,-0.0922024005987424,
-0.455300369321535));
#10121=CARTESIAN_POINT('Ctrl Pts',(7.19545310482183,-0.168916263556222,
-0.450067031743127));
#10122=CARTESIAN_POINT('Ctrl Pts',(7.26682926172338,-0.229429054168326,
-0.444833694164719));
#10123=CARTESIAN_POINT('Ctrl Pts',(7.3474407176227,-0.246609572473441,-0.43960035658631));
#10124=CARTESIAN_POINT('Ctrl Pts',(7.42805217352202,-0.263790090778555,
-0.434367019007902));
#10125=CARTESIAN_POINT('Ctrl Pts',(7.5178989284191,-0.237638336776682,-0.429133681429493));
#10126=CARTESIAN_POINT('Ctrl Pts',(7.57669775877139,-0.179879574833401,
-0.423900343851085));
#10127=CARTESIAN_POINT('Ctrl Pts',(7.63549658912369,-0.122120812890119,
-0.418667006272676));
#10128=CARTESIAN_POINT('Ctrl Pts',(7.66324749493119,-0.0327550430054262,
-0.413433668694268));
#10129=CARTESIAN_POINT('Ctrl Pts',(7.64750822446396,0.0481501632372987,
-0.408200331115859));
#10130=CARTESIAN_POINT('Ctrl Pts',(7.63176895399672,0.129055369480023,-0.402966993537451));
#10131=CARTESIAN_POINT('Ctrl Pts',(7.57253950725476,0.20150001208078,-0.397733655959043));
#10132=CARTESIAN_POINT('Ctrl Pts',(7.49637569079484,0.233003188011166,-0.392500318380634));
#10133=CARTESIAN_POINT('Ctrl Pts',(7.42021187433493,0.264506363941552,-0.387266980802226));
#10134=CARTESIAN_POINT('Ctrl Pts',(7.32711368815708,0.255068073201566,-0.382033643223817));
#10135=CARTESIAN_POINT('Ctrl Pts',(7.25882215060389,0.208920018748368,-0.376800305645409));
#10136=CARTESIAN_POINT('Ctrl Pts',(7.19121804006457,0.16323649358247,-0.371619647180005));
#10137=CARTESIAN_POINT('Ctrl Pts',(7.14792368105538,0.0815785307526936,
-0.366438988714602));
#10138=CARTESIAN_POINT('Ctrl Pts',(7.14785287490956,-1.4768633667023E-5,
-0.361258330249198));
#10139=CARTESIAN_POINT('Origin',(7.4,0.,-0.45));
#10140=CARTESIAN_POINT('',(7.14851414192891,0.000162483299119997,-0.261258330249198));
#10141=CARTESIAN_POINT('',(7.1486107370081,-8.15071611798959E-5,-0.288741669750802));
#10142=CARTESIAN_POINT('',(7.14825,3.08304831685346E-17,-0.45));
#10143=CARTESIAN_POINT('Ctrl Pts',(7.1486107370081,-8.15071611798959E-5,
-0.288741669750802));
#10144=CARTESIAN_POINT('Ctrl Pts',(7.14874995825962,0.0467834254920333,
-0.291694310658131));
#10145=CARTESIAN_POINT('Ctrl Pts',(7.16134085284144,0.0937178459994653,
-0.29464695156546));
#10146=CARTESIAN_POINT('Ctrl Pts',(7.18590655823031,0.133201931233131,-0.297599592472789));
#10147=CARTESIAN_POINT('Ctrl Pts',(7.22944745371562,0.203184551364662,-0.302832930051197));
#10148=CARTESIAN_POINT('Ctrl Pts',(7.31060714555302,0.249761987904173,-0.308066267629606));
#10149=CARTESIAN_POINT('Ctrl Pts',(7.39299729675863,0.252051023574679,-0.313299605208015));
#10150=CARTESIAN_POINT('Ctrl Pts',(7.47538744796424,0.254340059245185,-0.318532942786423));
#10151=CARTESIAN_POINT('Ctrl Pts',(7.55900805853805,0.212340694046686,-0.323766280364831));
#10152=CARTESIAN_POINT('Ctrl Pts',(7.60636742654168,0.144883544918643,-0.32899961794324));
#10153=CARTESIAN_POINT('Ctrl Pts',(7.6537267945453,0.0774263957905979,-0.334232955521648));
#10154=CARTESIAN_POINT('Ctrl Pts',(7.66482491997874,-0.0154885372669925,
-0.339466293100057));
#10155=CARTESIAN_POINT('Ctrl Pts',(7.63468590510707,-0.0922023983707198,
-0.344699630678465));
#10156=CARTESIAN_POINT('Ctrl Pts',(7.6045468902354,-0.168916259474447,-0.349932968256874));
#10157=CARTESIAN_POINT('Ctrl Pts',(7.53317073505863,-0.229429048624311,
-0.355166305835282));
#10158=CARTESIAN_POINT('Ctrl Pts',(7.45255928110724,-0.246609566514272,
-0.360399643413691));
#10159=CARTESIAN_POINT('Ctrl Pts',(7.37194782715585,-0.263790084404232,
-0.365632980992099));
#10160=CARTESIAN_POINT('Ctrl Pts',(7.28210107442985,-0.237638331034289,
-0.370866318570508));
#10161=CARTESIAN_POINT('Ctrl Pts',(7.2233022454984,-0.179879570486712,-0.376099656148916));
#10162=CARTESIAN_POINT('Ctrl Pts',(7.17595606765367,-0.133370879775126,
-0.380313660682878));
#10163=CARTESIAN_POINT('Ctrl Pts',(7.14874087646276,-0.0663687015160148,
-0.38452766521684));
#10164=CARTESIAN_POINT('Ctrl Pts',(7.14815269739345,0.000207923984461611,
-0.388741669750802));
#10165=CARTESIAN_POINT('Ctrl Pts',(7.14785287490956,-1.4768633667023E-5,
-0.361258330249198));
#10166=CARTESIAN_POINT('Ctrl Pts',(7.14785215492291,-0.000844443600183524,
-0.361205651136193));
#10167=CARTESIAN_POINT('Ctrl Pts',(7.14785590411212,-0.00167411188070867,
-0.361152972023188));
#10168=CARTESIAN_POINT('Ctrl Pts',(7.14786414236282,-0.00250373558438578,
-0.361100292910184));
#10169=CARTESIAN_POINT('Ctrl Pts',(7.14868256060344,-0.0849216172975351,
-0.355866955331775));
#10170=CARTESIAN_POINT('Ctrl Pts',(7.19380428601321,-0.166899562557425,
-0.350633617753366));
#10171=CARTESIAN_POINT('Ctrl Pts',(7.26299877655295,-0.21168236625759,-0.345400280174958));
#10172=CARTESIAN_POINT('Ctrl Pts',(7.33219326709269,-0.256465169957754,
-0.340166942596549));
#10173=CARTESIAN_POINT('Ctrl Pts',(7.42546052276241,-0.264052832098196,
-0.334933605018141));
#10174=CARTESIAN_POINT('Ctrl Pts',(7.50098372212563,-0.231043388201001,
-0.329700267439733));
#10175=CARTESIAN_POINT('Ctrl Pts',(7.57650692148885,-0.198033944303807,
-0.324466929861324));
#10176=CARTESIAN_POINT('Ctrl Pts',(7.63428606454555,-0.124427394368975,
-0.319233592282916));
#10177=CARTESIAN_POINT('Ctrl Pts',(7.64841559530002,-0.0432255876523345,
-0.314000254704507));
#10178=CARTESIAN_POINT('Ctrl Pts',(7.66254512605448,0.0379762190643056,
-0.308766917126099));
#10179=CARTESIAN_POINT('Ctrl Pts',(7.63302504450671,0.126773282562755,-0.303533579547691));
#10180=CARTESIAN_POINT('Ctrl Pts',(7.57309082092558,0.183353012510955,-0.298300241969282));
#10181=CARTESIAN_POINT('Ctrl Pts',(7.51315659734445,0.239932742459157,-0.293066904390874));
#10182=CARTESIAN_POINT('Ctrl Pts',(7.42280823172995,0.264295138857109,-0.287833566812465));
#10183=CARTESIAN_POINT('Ctrl Pts',(7.34255384697395,0.245517206379848,-0.282600229234057));
#10184=CARTESIAN_POINT('Ctrl Pts',(7.26229946221796,0.226739273902587,-0.277366891655648));
#10185=CARTESIAN_POINT('Ctrl Pts',(7.19213905832046,0.164821012550114,-0.27213355407724));
#10186=CARTESIAN_POINT('Ctrl Pts',(7.16352938934256,0.0875237678523623,
-0.266900216498831));
#10187=CARTESIAN_POINT('Ctrl Pts',(7.15324834685328,0.059746576244338,-0.265019587748954));
#10188=CARTESIAN_POINT('Ctrl Pts',(7.14833301628059,0.0299833982425618,
-0.263138958999076));
#10189=CARTESIAN_POINT('Ctrl Pts',(7.14851414192891,0.000162483299119997,
-0.261258330249198));
#10190=CARTESIAN_POINT('Origin',(7.4,0.,-0.45));
#10191=CARTESIAN_POINT('',(7.1483354802531,-0.000213511019231185,-0.161258330249198));
#10192=CARTESIAN_POINT('',(7.14789741337032,-9.36993803829212E-5,-0.188741669750802));
#10193=CARTESIAN_POINT('',(7.14825,3.08304831685346E-17,-0.45));
#10194=CARTESIAN_POINT('Ctrl Pts',(7.14789741337032,-9.36993803829212E-5,
-0.188741669750802));
#10195=CARTESIAN_POINT('Ctrl Pts',(7.14827035947299,0.0768944579770298,
-0.193627618521014));
#10196=CARTESIAN_POINT('Ctrl Pts',(7.18617228508483,0.154200799589981,-0.198513567291225));
#10197=CARTESIAN_POINT('Ctrl Pts',(7.24744009054551,0.200759129579989,-0.203399516061437));
#10198=CARTESIAN_POINT('Ctrl Pts',(7.31306401002228,0.250627736350931,-0.208632853639845));
#10199=CARTESIAN_POINT('Ctrl Pts',(7.40549453487257,0.2652205555663,-0.213866191218254));
#10200=CARTESIAN_POINT('Ctrl Pts',(7.48329000647319,0.23799481444734,-0.219099528796662));
#10201=CARTESIAN_POINT('Ctrl Pts',(7.56108547807381,0.21076907332838,-0.224332866375071));
#10202=CARTESIAN_POINT('Ctrl Pts',(7.62424589642476,0.141724771875092,-0.229566203953479));
#10203=CARTESIAN_POINT('Ctrl Pts',(7.64445297975488,0.061818259925214,-0.234799541531888));
#10204=CARTESIAN_POINT('Ctrl Pts',(7.66466006308499,-0.0180882520246644,
-0.240032879110296));
#10205=CARTESIAN_POINT('Ctrl Pts',(7.64191381139426,-0.108856974471133,
-0.245266216688705));
#10206=CARTESIAN_POINT('Ctrl Pts',(7.58641261833332,-0.169791318327095,
-0.250499554267113));
#10207=CARTESIAN_POINT('Ctrl Pts',(7.53091142527237,-0.230725662183056,
-0.255732891845522));
#10208=CARTESIAN_POINT('Ctrl Pts',(7.4426552908412,-0.261825627448513,-0.26096622942393));
#10209=CARTESIAN_POINT('Ctrl Pts',(7.36121427497037,-0.24914739401983,-0.266199567002338));
#10210=CARTESIAN_POINT('Ctrl Pts',(7.27977325909954,-0.236469160591147,
-0.271432904580747));
#10211=CARTESIAN_POINT('Ctrl Pts',(7.20514736178904,-0.180012728468324,
-0.276666242159155));
#10212=CARTESIAN_POINT('Ctrl Pts',(7.1707954627004,-0.105090610545136,-0.281899579737564));
#10213=CARTESIAN_POINT('Ctrl Pts',(7.15582485155161,-0.0724394348131096,
-0.284180276408643));
#10214=CARTESIAN_POINT('Ctrl Pts',(7.14850319889059,-0.0362812006719064,
-0.286460973079723));
#10215=CARTESIAN_POINT('Ctrl Pts',(7.1486107370081,-8.15071611798959E-5,
-0.288741669750802));
#10216=CARTESIAN_POINT('Ctrl Pts',(7.14851414192891,0.000162483299119997,
-0.261258330249198));
#10217=CARTESIAN_POINT('Ctrl Pts',(7.1488370454048,-0.0530010370459997,
-0.257905621420668));
#10218=CARTESIAN_POINT('Ctrl Pts',(7.16535766681591,-0.106348058760499,
-0.254552912592137));
#10219=CARTESIAN_POINT('Ctrl Pts',(7.19655039731096,-0.148953076906415,
-0.251200203763606));
#10220=CARTESIAN_POINT('Ctrl Pts',(7.24524000831559,-0.21545644892441,-0.245966866185198));
#10221=CARTESIAN_POINT('Ctrl Pts',(7.32967816438315,-0.255786964917369,
-0.240733528606789));
#10222=CARTESIAN_POINT('Ctrl Pts',(7.41200661495652,-0.251862260678651,
-0.235500191028381));
#10223=CARTESIAN_POINT('Ctrl Pts',(7.49433506552989,-0.247937556439932,
-0.230266853449972));
#10224=CARTESIAN_POINT('Ctrl Pts',(7.57455381060907,-0.199757631969536,
-0.225033515871564));
#10225=CARTESIAN_POINT('Ctrl Pts',(7.61669638752149,-0.128924155045882,
-0.219800178293155));
#10226=CARTESIAN_POINT('Ctrl Pts',(7.65883896443392,-0.0580906781222288,
-0.214566840714747));
#10227=CARTESIAN_POINT('Ctrl Pts',(7.66290537317959,0.0353963512546822,
-0.209333503136338));
#10228=CARTESIAN_POINT('Ctrl Pts',(7.62707242700085,0.109621509538064,-0.20410016555793));
#10229=CARTESIAN_POINT('Ctrl Pts',(7.59123948082212,0.183846667821447,-0.198866827979521));
#10230=CARTESIAN_POINT('Ctrl Pts',(7.51550717971897,0.238809955011301,-0.193633490401113));
#10231=CARTESIAN_POINT('Ctrl Pts',(7.43383044982246,0.249868449747252,-0.188400152822705));
#10232=CARTESIAN_POINT('Ctrl Pts',(7.35215371992594,0.260926944483204,-0.183166815244296));
#10233=CARTESIAN_POINT('Ctrl Pts',(7.26453256123606,0.228080646765252,-0.177933477665888));
#10234=CARTESIAN_POINT('Ctrl Pts',(7.2102523694764,0.166056085274717,-0.172700140087479));
#10235=CARTESIAN_POINT('Ctrl Pts',(7.17069420843708,0.120854004878616,-0.168886203474719));
#10236=CARTESIAN_POINT('Ctrl Pts',(7.14884397070955,0.0601548797106173,
-0.165072266861959));
#10237=CARTESIAN_POINT('Ctrl Pts',(7.1483354802531,-0.000213511019231185,
-0.161258330249198));
#10238=CARTESIAN_POINT('Origin',(7.4,0.,-0.45));
#10239=CARTESIAN_POINT('',(7.14794643808389,0.00012639595204536,-0.0612583302491982));
#10240=CARTESIAN_POINT('',(7.14840641220525,0.000201202115797984,-0.0887416697508019));
#10241=CARTESIAN_POINT('',(7.14825,3.08304831685346E-17,-0.45));
#10242=CARTESIAN_POINT('',(7.59134659966651,0.163598720337495,0.));
#10243=CARTESIAN_POINT('Ctrl Pts',(7.14794643808389,0.00012639595204536,
-0.0612583302491982));
#10244=CARTESIAN_POINT('Ctrl Pts',(7.14842546082296,-0.0742619964396601,
-0.0565388995680243));
#10245=CARTESIAN_POINT('Ctrl Pts',(7.18347141764068,-0.149027219123109,
-0.0518194688868503));
#10246=CARTESIAN_POINT('Ctrl Pts',(7.24121260951448,-0.195852567382474,
-0.0471000382056764));
#10247=CARTESIAN_POINT('Ctrl Pts',(7.3052413387552,-0.247776808084922,-0.0418667006272679));
#10248=CARTESIAN_POINT('Ctrl Pts',(7.39717705575739,-0.265345038299558,
-0.0366333630488594));
#10249=CARTESIAN_POINT('Ctrl Pts',(7.47578474042289,-0.240530500580791,
-0.0314000254704509));
#10250=CARTESIAN_POINT('Ctrl Pts',(7.55439242508838,-0.215715962862024,
-0.0261666878920425));
#10251=CARTESIAN_POINT('Ctrl Pts',(7.61967207741718,-0.148518657209854,
-0.020933350313634));
#10252=CARTESIAN_POINT('Ctrl Pts',(7.64235926604704,-0.0694196478813939,
-0.0157000127352255));
#10253=CARTESIAN_POINT('Ctrl Pts',(7.66504645467691,0.00967936144706648,
-0.010466675156817));
#10254=CARTESIAN_POINT('Ctrl Pts',(7.64514117960785,0.100680074451818,-0.00523333757840849));
#10255=CARTESIAN_POINT('Ctrl Pts',(7.59134659966651,0.163598720337495,0.));
#10256=CARTESIAN_POINT('',(7.20829763049428,0.163827060994237,1.44778665420313E-16));
#10257=CARTESIAN_POINT('Origin',(7.4,0.,0.));
#10258=CARTESIAN_POINT('Ctrl Pts',(7.20829596415884,0.1638281304838,9.0205620750794E-17));
#10259=CARTESIAN_POINT('Ctrl Pts',(7.2596674427612,0.223538347845456,-0.00499978774624422));
#10260=CARTESIAN_POINT('Ctrl Pts',(7.3414071265269,0.257577506526122,-0.00999957549248853));
#10261=CARTESIAN_POINT('Ctrl Pts',(7.41991797435699,0.25134623940458,-0.0149993632387328));
#10262=CARTESIAN_POINT('Ctrl Pts',(7.50209621693749,0.24482389764862,-0.0202327008171413));
#10263=CARTESIAN_POINT('Ctrl Pts',(7.58073692780066,0.19418103958705,-0.0254660383955497));
#10264=CARTESIAN_POINT('Ctrl Pts',(7.62062911488364,0.122067692861168,-0.0306993759739582));
#10265=CARTESIAN_POINT('Ctrl Pts',(7.66052130196662,0.049954346135286,-0.0359327135523666));
#10266=CARTESIAN_POINT('Ctrl Pts',(7.6616649652694,-0.0436294892549086,
-0.0411660511307751));
#10267=CARTESIAN_POINT('Ctrl Pts',(7.62352358784103,-0.116697418725104,
-0.0463993887091835));
#10268=CARTESIAN_POINT('Ctrl Pts',(7.58538221041266,-0.1897653481953,-0.051632726287592));
#10269=CARTESIAN_POINT('Ctrl Pts',(7.50795579225314,-0.242317371745497,
-0.0568660638660004));
#10270=CARTESIAN_POINT('Ctrl Pts',(7.42597061249076,-0.250805231205967,
-0.0620994014444088));
#10271=CARTESIAN_POINT('Ctrl Pts',(7.34398543272838,-0.259293090666436,
-0.0673327390228173));
#10272=CARTESIAN_POINT('Ctrl Pts',(7.25744149136314,-0.223716786037178,
-0.0725660766012258));
#10273=CARTESIAN_POINT('Ctrl Pts',(7.20513534285944,-0.160020335565283,
-0.0777994141796342));
#10274=CARTESIAN_POINT('Ctrl Pts',(7.16868013390367,-0.11562656010828,-0.0814468327033568));
#10275=CARTESIAN_POINT('Ctrl Pts',(7.14885596689451,-0.0575733958307166,
-0.0850942512270793));
#10276=CARTESIAN_POINT('Ctrl Pts',(7.14840641220525,0.000201202115797984,
-0.0887416697508019));
#10277=CARTESIAN_POINT('Origin',(-7.4,0.,-0.45));
#10278=CARTESIAN_POINT('',(-7.65135844136173,-9.87909931464411E-6,-0.761258330249198));
#10279=CARTESIAN_POINT('',(-7.6515844849848,-0.000333784136707353,-0.788741669750802));
#10280=CARTESIAN_POINT('',(-7.65175,3.08304831685346E-17,-0.45));
#10281=CARTESIAN_POINT('',(-7.59134659966651,0.163598720337494,-0.8));
#10282=CARTESIAN_POINT('Ctrl Pts',(-7.6515844849848,-0.000333784136707353,
-0.788741669750802));
#10283=CARTESIAN_POINT('Ctrl Pts',(-7.65107118775856,0.0589216006363537,
-0.792494446500534));
#10284=CARTESIAN_POINT('Ctrl Pts',(-7.62992218280841,0.118480356030438,
-0.796247223250267));
#10285=CARTESIAN_POINT('Ctrl Pts',(-7.59134659966651,0.163598720337491,
-0.8));
#10286=CARTESIAN_POINT('',(-7.20829765525586,0.163827077455369,-0.799999999999998));
#10287=CARTESIAN_POINT('Origin',(-7.4,0.,-0.8));
#10288=CARTESIAN_POINT('Ctrl Pts',(-7.2082959906101,0.163828146011844,-0.799999999999999));
#10289=CARTESIAN_POINT('Ctrl Pts',(-7.25966747611426,0.22353839593213,-0.795000212253755));
#10290=CARTESIAN_POINT('Ctrl Pts',(-7.34140714099376,0.257577466209252,
-0.790000424507512));
#10291=CARTESIAN_POINT('Ctrl Pts',(-7.4199179741645,0.251346180862741,-0.785000636761268));
#10292=CARTESIAN_POINT('Ctrl Pts',(-7.50209620140088,0.244823820030488,
-0.779767299182859));
#10293=CARTESIAN_POINT('Ctrl Pts',(-7.58073690155091,0.194181019780683,
-0.77453396160445));
#10294=CARTESIAN_POINT('Ctrl Pts',(-7.62062908494217,0.122067693270255,
-0.769300624026042));
#10295=CARTESIAN_POINT('Ctrl Pts',(-7.64106375997351,0.0851278151438433,
-0.76661985943376));
#10296=CARTESIAN_POINT('Ctrl Pts',(-7.65133091722897,0.0425541224698544,
-0.763939094841479));
#10297=CARTESIAN_POINT('Ctrl Pts',(-7.65135844136173,-9.87909931464411E-6,
-0.761258330249198));
#10298=CARTESIAN_POINT('Origin',(-7.4,0.,-0.45));
#10299=CARTESIAN_POINT('',(-7.65201712840627,-0.000154017282173287,-0.661258330249199));
#10300=CARTESIAN_POINT('',(-7.65207346276915,0.000120387280643822,-0.688741669750802));
#10301=CARTESIAN_POINT('',(-7.65175,3.08304831685346E-17,-0.45));
#10302=CARTESIAN_POINT('Ctrl Pts',(-7.65207346276915,0.000120387280643822,
-0.688741669750802));
#10303=CARTESIAN_POINT('Ctrl Pts',(-7.65211569074847,0.00725647012215086,
-0.689194416785009));
#10304=CARTESIAN_POINT('Ctrl Pts',(-7.65183830629956,0.014389201188033,
-0.689647163819216));
#10305=CARTESIAN_POINT('Ctrl Pts',(-7.65123053408043,0.0214936402840764,
-0.690099910853423));
#10306=CARTESIAN_POINT('Ctrl Pts',(-7.64420524853858,0.103614394890392,
-0.695333248431831));
#10307=CARTESIAN_POINT('Ctrl Pts',(-7.59303611022166,0.181954995799164,
-0.700566586010239));
#10308=CARTESIAN_POINT('Ctrl Pts',(-7.52066407726933,0.221399944694366,
-0.705799923588648));
#10309=CARTESIAN_POINT('Ctrl Pts',(-7.44829204431699,0.260844893589568,
-0.711033261167056));
#10310=CARTESIAN_POINT('Ctrl Pts',(-7.35471711672925,0.261394190471199,
-0.716266598745465));
#10311=CARTESIAN_POINT('Ctrl Pts',(-7.2818960197261,0.222783627398016,-0.721499936323873));
#10312=CARTESIAN_POINT('Ctrl Pts',(-7.20907492272296,0.184173064324832,
-0.726733273902282));
#10313=CARTESIAN_POINT('Ctrl Pts',(-7.15700765630441,0.106402641296834,
-0.73196661148069));
#10314=CARTESIAN_POINT('Ctrl Pts',(-7.14903488410923,0.0243772822946468,
-0.737199949059099));
#10315=CARTESIAN_POINT('Ctrl Pts',(-7.14106211191404,-0.0576480767075406,
-0.742433286637507));
#10316=CARTESIAN_POINT('Ctrl Pts',(-7.17718383394222,-0.143928371683915,
-0.747666624215915));
#10317=CARTESIAN_POINT('Ctrl Pts',(-7.24121258230851,-0.195852606685422,
-0.752899961794324));
#10318=CARTESIAN_POINT('Ctrl Pts',(-7.3052413306748,-0.247776841686928,
-0.758133299372732));
#10319=CARTESIAN_POINT('Ctrl Pts',(-7.3971771053792,-0.265345016713566,
-0.763366636951141));
#10320=CARTESIAN_POINT('Ctrl Pts',(-7.47578476199579,-0.240530505659223,
-0.768599974529549));
#10321=CARTESIAN_POINT('Ctrl Pts',(-7.55439241861237,-0.215715994604879,
-0.773833312107958));
#10322=CARTESIAN_POINT('Ctrl Pts',(-7.61967195714114,-0.148518797469554,
-0.779066649686366));
#10323=CARTESIAN_POINT('Ctrl Pts',(-7.64235914739001,-0.0694197802053813,
-0.784299987264774));
#10324=CARTESIAN_POINT('Ctrl Pts',(-7.64877756865406,-0.0470419181253069,
-0.78578054809345));
#10325=CARTESIAN_POINT('Ctrl Pts',(-7.65178699310541,-0.0237114608368644,
-0.787261108922126));
#10326=CARTESIAN_POINT('Ctrl Pts',(-7.6515844849848,-0.000333784136707353,
-0.788741669750802));
#10327=CARTESIAN_POINT('Ctrl Pts',(-7.65135844136173,-9.87909931464411E-6,
-0.761258330249198));
#10328=CARTESIAN_POINT('Ctrl Pts',(-7.65138464931672,-0.040538510706789,
-0.758705757263071));
#10329=CARTESIAN_POINT('Ctrl Pts',(-7.64212710855812,-0.0810583558879505,
-0.756153184276944));
#10330=CARTESIAN_POINT('Ctrl Pts',(-7.62352356237588,-0.116697412903133,
-0.753600611290817));
#10331=CARTESIAN_POINT('Ctrl Pts',(-7.58538218978582,-0.189765339795041,
-0.748367273712409));
#10332=CARTESIAN_POINT('Ctrl Pts',(-7.50795577797319,-0.242317340807806,
-0.743133936134));
#10333=CARTESIAN_POINT('Ctrl Pts',(-7.42597060788136,-0.250805195601303,
-0.737900598555591));
#10334=CARTESIAN_POINT('Ctrl Pts',(-7.34398543778953,-0.2592930503948,-0.732667260977183));
#10335=CARTESIAN_POINT('Ctrl Pts',(-7.25744150941849,-0.22371675896903,
-0.727433923398775));
#10336=CARTESIAN_POINT('Ctrl Pts',(-7.20513536776807,-0.160020318362261,
-0.722200585820366));
#10337=CARTESIAN_POINT('Ctrl Pts',(-7.15282922611764,-0.0963238777554929,
-0.716967248241958));
#10338=CARTESIAN_POINT('Ctrl Pts',(-7.13476087118783,-0.00450728796772577,
-0.711733910663549));
#10339=CARTESIAN_POINT('Ctrl Pts',(-7.15903423279356,0.0742596685861753,
-0.706500573085141));
#10340=CARTESIAN_POINT('Ctrl Pts',(-7.1833075943993,0.153026625140077,-0.701267235506732));
#10341=CARTESIAN_POINT('Ctrl Pts',(-7.24992267254058,0.218743948460114,
-0.696033897928324));
#10342=CARTESIAN_POINT('Ctrl Pts',(-7.32901084118502,0.241948634523276,
-0.690800560349916));
#10343=CARTESIAN_POINT('Ctrl Pts',(-7.40809900982946,0.265153320586438,
-0.685567222771507));
#10344=CARTESIAN_POINT('Ctrl Pts',(-7.49966026897706,0.245845369392726,
-0.680333885193098));
#10345=CARTESIAN_POINT('Ctrl Pts',(-7.56264340109525,0.192680763788563,
-0.67510054761469));
#10346=CARTESIAN_POINT('Ctrl Pts',(-7.61817368758881,0.145807169522468,
-0.670486475159526));
#10347=CARTESIAN_POINT('Ctrl Pts',(-7.65148903726443,0.0726154250913533,
-0.665872402704363));
#10348=CARTESIAN_POINT('Ctrl Pts',(-7.65201712840627,-0.000154017282173287,
-0.661258330249199));
#10349=CARTESIAN_POINT('Origin',(-7.4,0.,-0.45));
#10350=CARTESIAN_POINT('',(-7.65171164790384,0.000216666439528223,-0.561258330249198));
#10351=CARTESIAN_POINT('',(-7.6513752928688,5.66816418782093E-5,-0.588741669750802));
#10352=CARTESIAN_POINT('',(-7.65175,3.08304831685346E-17,-0.45));
#10353=CARTESIAN_POINT('Ctrl Pts',(-7.6513752928688,5.66816418782093E-5,
-0.588741669750802));
#10354=CARTESIAN_POINT('Ctrl Pts',(-7.65145324746199,0.0379339415427937,
-0.591127724647891));
#10355=CARTESIAN_POINT('Ctrl Pts',(-7.64340989881181,0.0757797670326688,
-0.593513779544981));
#10356=CARTESIAN_POINT('Ctrl Pts',(-7.62707244990212,0.109621520545763,
-0.59589983444207));
#10357=CARTESIAN_POINT('Ctrl Pts',(-7.59123950011597,0.183846686360407,
-0.601133172020479));
#10358=CARTESIAN_POINT('Ctrl Pts',(-7.51550719140105,0.238809979279913,
-0.606366509598887));
#10359=CARTESIAN_POINT('Ctrl Pts',(-7.43383045324891,0.249868475051116,
-0.611599847177296));
#10360=CARTESIAN_POINT('Ctrl Pts',(-7.35215371509677,0.260926970822319,
-0.616833184755704));
#10361=CARTESIAN_POINT('Ctrl Pts',(-7.2645325475074,0.22808066944522,-0.622066522334113));
#10362=CARTESIAN_POINT('Ctrl Pts',(-7.21025235030538,0.166056101845713,
-0.627299859912521));
#10363=CARTESIAN_POINT('Ctrl Pts',(-7.15597215310335,0.104031534246204,
-0.63253319749093));
#10364=CARTESIAN_POINT('Ctrl Pts',(-7.13503292628866,0.0128287004242853,
-0.637766535069338));
#10365=CARTESIAN_POINT('Ctrl Pts',(-7.15682281406447,-0.0666606352401807,
-0.642999872647747));
#10366=CARTESIAN_POINT('Ctrl Pts',(-7.17861270184028,-0.146149970904647,
-0.648233210226155));
#10367=CARTESIAN_POINT('Ctrl Pts',(-7.24313170420659,-0.21392580841166,
-0.653466547804563));
#10368=CARTESIAN_POINT('Ctrl Pts',(-7.32145253515356,-0.23960160800038,
-0.658699885382972));
#10369=CARTESIAN_POINT('Ctrl Pts',(-7.39977336610052,-0.2652774075891,-0.66393322296138));
#10370=CARTESIAN_POINT('Ctrl Pts',(-7.49189602562815,-0.248853169259528,
-0.669166560539789));
#10371=CARTESIAN_POINT('Ctrl Pts',(-7.55651663900859,-0.197690595942813,
-0.674399898118197));
#10372=CARTESIAN_POINT('Ctrl Pts',(-7.61554678729514,-0.150954204385727,
-0.679180488662399));
#10373=CARTESIAN_POINT('Ctrl Pts',(-7.65162757430742,-0.0752300569569674,
-0.6839610792066));
#10374=CARTESIAN_POINT('Ctrl Pts',(-7.65207346276915,0.000120387280643822,
-0.688741669750802));
#10375=CARTESIAN_POINT('Ctrl Pts',(-7.65201712840627,-0.000154017282173287,
-0.661258330249199));
#10376=CARTESIAN_POINT('Ctrl Pts',(-7.65208800471547,-0.00992056909464737,
-0.660639065125954));
#10377=CARTESIAN_POINT('Ctrl Pts',(-7.65156828634817,-0.0196795140086419,
-0.66001980000271));
#10378=CARTESIAN_POINT('Ctrl Pts',(-7.65043241411917,-0.0293662054698359,
-0.659400534879465));
#10379=CARTESIAN_POINT('Ctrl Pts',(-7.6408332899361,-0.11122730910946,-0.654167197301057));
#10380=CARTESIAN_POINT('Ctrl Pts',(-7.58723003648116,-0.187928256374095,
-0.648933859722648));
#10381=CARTESIAN_POINT('Ctrl Pts',(-7.5136561047022,-0.225080013667832,
-0.643700522144239));
#10382=CARTESIAN_POINT('Ctrl Pts',(-7.44008217292323,-0.26223177096157,
-0.638467184565831));
#10383=CARTESIAN_POINT('Ctrl Pts',(-7.34653756282023,-0.25983433828441,
-0.633233846987423));
#10384=CARTESIAN_POINT('Ctrl Pts',(-7.27496336219634,-0.218962514901155,
-0.628000509409015));
#10385=CARTESIAN_POINT('Ctrl Pts',(-7.20338916157245,-0.178090691517901,
-0.622767171830606));
#10386=CARTESIAN_POINT('Ctrl Pts',(-7.15378537042767,-0.0987444774285509,
-0.617533834252197));
#10387=CARTESIAN_POINT('Ctrl Pts',(-7.14839212952851,-0.0164991784990361,
-0.612300496673789));
#10388=CARTESIAN_POINT('Ctrl Pts',(-7.14299888862934,0.0657461204304788,
-0.60706715909538));
#10389=CARTESIAN_POINT('Ctrl Pts',(-7.1818161979758,0.150890504200159,-0.601833821516972));
#10390=CARTESIAN_POINT('Ctrl Pts',(-7.24744010936701,0.200759104807884,
-0.596600483938564));
#10391=CARTESIAN_POINT('Ctrl Pts',(-7.31306402075823,0.250627705415608,
-0.591367146360155));
#10392=CARTESIAN_POINT('Ctrl Pts',(-7.40549453419421,0.265220522861378,
-0.586133808781746));
#10393=CARTESIAN_POINT('Ctrl Pts',(-7.4832899961977,0.23799478510693,-0.580900471203338));
#10394=CARTESIAN_POINT('Ctrl Pts',(-7.56108545820118,0.210769047352483,
-0.575667133624929));
#10395=CARTESIAN_POINT('Ctrl Pts',(-7.62424586877218,0.141724754397818,
-0.570433796046521));
#10396=CARTESIAN_POINT('Ctrl Pts',(-7.64445294961248,0.0618182522979024,
-0.565200458468113));
#10397=CARTESIAN_POINT('Ctrl Pts',(-7.64952676101288,0.0417544675026141,
-0.563886415728475));
#10398=CARTESIAN_POINT('Ctrl Pts',(-7.65189251219152,0.0210058576497331,
-0.562572372988837));
#10399=CARTESIAN_POINT('Ctrl Pts',(-7.65171164790384,0.000216666439528223,
-0.561258330249198));
#10400=CARTESIAN_POINT('Origin',(-7.4,0.,-0.45));
#10401=CARTESIAN_POINT('',(-7.65145417026957,-0.000143789196739241,-0.461258330249198));
#10402=CARTESIAN_POINT('',(-7.65189502578968,-0.000198275244604145,-0.488741669750802));
#10403=CARTESIAN_POINT('',(-7.65175,3.08304831685346E-17,-0.45));
#10404=CARTESIAN_POINT('Ctrl Pts',(-7.65189502578968,-0.000198275244604145,
-0.488741669750802));
#10405=CARTESIAN_POINT('Ctrl Pts',(-7.65130644308897,0.068009450109477,
-0.493061032510774));
#10406=CARTESIAN_POINT('Ctrl Pts',(-7.62255787077756,0.13665464789974,-0.497380395270746));
#10407=CARTESIAN_POINT('Ctrl Pts',(-7.57309083838734,0.183353031006997,
-0.501699758030718));
#10408=CARTESIAN_POINT('Ctrl Pts',(-7.51315660875997,0.239932766664044,
-0.506933095609127));
#10409=CARTESIAN_POINT('Ctrl Pts',(-7.4228082340312,0.264295165523682,-0.512166433187536));
#10410=CARTESIAN_POINT('Ctrl Pts',(-7.34255384117878,0.245517231150252,
-0.517399770765944));
#10411=CARTESIAN_POINT('Ctrl Pts',(-7.26229944832636,0.226739296776823,
-0.522633108344353));
#10412=CARTESIAN_POINT('Ctrl Pts',(-7.19213903735029,0.164821029170327,
-0.527866445922761));
#10413=CARTESIAN_POINT('Ctrl Pts',(-7.16352936548653,0.0875237766780772,
-0.533099783501169));
#10414=CARTESIAN_POINT('Ctrl Pts',(-7.13491969362278,0.0102265241858273,
-0.538333121079577));
#10415=CARTESIAN_POINT('Ctrl Pts',(-7.14786076087134,-0.0824497131921767,
-0.543566458657986));
#10416=CARTESIAN_POINT('Ctrl Pts',(-7.19655037678711,-0.148953091925709,
-0.548799796236394));
#10417=CARTESIAN_POINT('Ctrl Pts',(-7.24523999270288,-0.215456470659241,
-0.554033133814803));
#10418=CARTESIAN_POINT('Ctrl Pts',(-7.32967815728587,-0.255786990748301,
-0.559266471393211));
#10419=CARTESIAN_POINT('Ctrl Pts',(-7.41200661616639,-0.251862286101345,
-0.56449980897162));
#10420=CARTESIAN_POINT('Ctrl Pts',(-7.49433507504691,-0.247937581454389,
-0.569733146550028));
#10421=CARTESIAN_POINT('Ctrl Pts',(-7.57455382822498,-0.199757652071417,
-0.574966484128437));
#10422=CARTESIAN_POINT('Ctrl Pts',(-7.61669640938532,-0.12892416802504,
-0.580199821706845));
#10423=CARTESIAN_POINT('Ctrl Pts',(-7.63962476814035,-0.090386055518247,
-0.583047104388164));
#10424=CARTESIAN_POINT('Ctrl Pts',(-7.65128226954256,-0.0451423061363344,
-0.585894387069483));
#10425=CARTESIAN_POINT('Ctrl Pts',(-7.6513752928688,5.66816418782093E-5,
-0.588741669750802));
#10426=CARTESIAN_POINT('Ctrl Pts',(-7.65171164790384,0.000216666439528223,
-0.561258330249198));
#10427=CARTESIAN_POINT('Ctrl Pts',(-7.65117219781758,-0.0617896651313866,
-0.557339035410428));
#10428=CARTESIAN_POINT('Ctrl Pts',(-7.62797794621862,-0.124157010215117,
-0.553419740571658));
#10429=CARTESIAN_POINT('Ctrl Pts',(-7.58641259534448,-0.169791297387043,
-0.549500445732887));
#10430=CARTESIAN_POINT('Ctrl Pts',(-7.5309114091266,-0.23072563372691,-0.544267108154479));
#10431=CARTESIAN_POINT('Ctrl Pts',(-7.44265528558124,-0.261825595161477,
-0.539033770576071));
#10432=CARTESIAN_POINT('Ctrl Pts',(-7.36121427975392,-0.249147363297231,
-0.533800432997662));
#10433=CARTESIAN_POINT('Ctrl Pts',(-7.2797732739266,-0.236469131432985,
-0.528567095419254));
#10434=CARTESIAN_POINT('Ctrl Pts',(-7.20514738581732,-0.180012706269927,
-0.523333757840845));
#10435=CARTESIAN_POINT('Ctrl Pts',(-7.1707954909645,-0.105090597585267,
-0.518100420262437));
#10436=CARTESIAN_POINT('Ctrl Pts',(-7.13644359611167,-0.0301684889006052,
-0.512867082684028));
#10437=CARTESIAN_POINT('Ctrl Pts',(-7.14236569451531,0.0632193033056596,
-0.50763374510562));
#10438=CARTESIAN_POINT('Ctrl Pts',(-7.18590658463152,0.133201914806981,
-0.502400407527211));
#10439=CARTESIAN_POINT('Ctrl Pts',(-7.22944747474773,0.203184526308302,
-0.497167069948803));
#10440=CARTESIAN_POINT('Ctrl Pts',(-7.31060715657653,0.24976195710468,-0.491933732370395));
#10441=CARTESIAN_POINT('Ctrl Pts',(-7.39299729762207,0.252050992493053,
-0.486700394791986));
#10442=CARTESIAN_POINT('Ctrl Pts',(-7.47538743866762,0.254340027881427,
-0.481467057213578));
#10443=CARTESIAN_POINT('Ctrl Pts',(-7.55900803892991,0.212340667861795,
-0.476233719635169));
#10444=CARTESIAN_POINT('Ctrl Pts',(-7.60636740109344,0.144883527052185,
-0.471000382056761));
#10445=CARTESIAN_POINT('Ctrl Pts',(-7.6357544702348,0.103025538040317,-0.46775303145424));
#10446=CARTESIAN_POINT('Ctrl Pts',(-7.65117967263087,0.0513653977049828,
-0.464505680851719));
#10447=CARTESIAN_POINT('Ctrl Pts',(-7.65145417026957,-0.000143789196739241,
-0.461258330249198));
#10448=CARTESIAN_POINT('Origin',(-7.4,0.,-0.45));
#10449=CARTESIAN_POINT('',(-7.65214708790382,-1.47686313733716E-5,-0.361258330249198));
#10450=CARTESIAN_POINT('',(-7.65184733409926,0.000207924010478792,-0.388741669750802));
#10451=CARTESIAN_POINT('',(-7.65175,3.08304831685346E-17,-0.45));
#10452=CARTESIAN_POINT('Ctrl Pts',(-7.65184733409926,0.000207924010478792,
-0.388741669750802));
#10453=CARTESIAN_POINT('Ctrl Pts',(-7.65198960979724,0.0163122642644074,
-0.389761002795248));
#10454=CARTESIAN_POINT('Ctrl Pts',(-7.65057389537345,0.0323917047289323,
-0.390780335839695));
#10455=CARTESIAN_POINT('Ctrl Pts',(-7.64750824943319,0.0481501680948176,
-0.391799668884141));
#10456=CARTESIAN_POINT('Ctrl Pts',(-7.63176897737814,0.129055382499451,
-0.39703300646255));
#10457=CARTESIAN_POINT('Ctrl Pts',(-7.57253952466095,0.201500032408553,
-0.402266344040958));
#10458=CARTESIAN_POINT('Ctrl Pts',(-7.49637570051745,0.233003211517073,
-0.407499681619367));
#10459=CARTESIAN_POINT('Ctrl Pts',(-7.42021187637395,0.264506390625591,
-0.412733019197775));
#10460=CARTESIAN_POINT('Ctrl Pts',(-7.32711368080414,0.255068098933529,
-0.417966356776183));
#10461=CARTESIAN_POINT('Ctrl Pts',(-7.25882213636153,0.208920039824769,
-0.423199694354592));
#10462=CARTESIAN_POINT('Ctrl Pts',(-7.19053059191893,0.162771980716008,
-0.428433031933));
#10463=CARTESIAN_POINT('Ctrl Pts',(-7.14704569860354,0.0799141541905499,
-0.433666369511409));
#10464=CARTESIAN_POINT('Ctrl Pts',(-7.14786411692674,-0.00250373583704704,
-0.438899707089817));
#10465=CARTESIAN_POINT('Ctrl Pts',(-7.14868253524993,-0.0849216258646429,
-0.444133044668226));
#10466=CARTESIAN_POINT('Ctrl Pts',(-7.1938042652117,-0.166899579394378,
-0.449366382246634));
#10467=CARTESIAN_POINT('Ctrl Pts',(-7.26299876273194,-0.211682387612474,
-0.454599719825042));
#10468=CARTESIAN_POINT('Ctrl Pts',(-7.33219326025219,-0.256465195830571,
-0.459833057403451));
#10469=CARTESIAN_POINT('Ctrl Pts',(-7.4254605253309,-0.264052858737029,
-0.465066394981859));
#10470=CARTESIAN_POINT('Ctrl Pts',(-7.5009837323131,-0.231043411509504,
-0.470299732560268));
#10471=CARTESIAN_POINT('Ctrl Pts',(-7.57650693929529,-0.19803396428198,
-0.475533070138676));
#10472=CARTESIAN_POINT('Ctrl Pts',(-7.63428608818096,-0.124427406920472,
-0.480766407717085));
#10473=CARTESIAN_POINT('Ctrl Pts',(-7.64841562036082,-0.0432255920124892,
-0.485999745295493));
#10474=CARTESIAN_POINT('Ctrl Pts',(-7.65088326866655,-0.0290441231266644,
-0.48691372011393));
#10475=CARTESIAN_POINT('Ctrl Pts',(-7.65201956957008,-0.0146309929533726,
-0.487827694932366));
#10476=CARTESIAN_POINT('Ctrl Pts',(-7.65189502578968,-0.000198275244604145,
-0.488741669750802));
#10477=CARTESIAN_POINT('Ctrl Pts',(-7.65145417026957,-0.000143789196739241,
-0.461258330249198));
#10478=CARTESIAN_POINT('Ctrl Pts',(-7.6516220451935,-0.0316453382582933,
-0.459272343273311));
#10479=CARTESIAN_POINT('Ctrl Pts',(-7.64612325866364,-0.0630904277678157,
-0.457286356297423));
#10480=CARTESIAN_POINT('Ctrl Pts',(-7.63468587616665,-0.0922023870006976,
-0.455300369321535));
#10481=CARTESIAN_POINT('Ctrl Pts',(-7.60454686501157,-0.168916238644387,
-0.450067031743127));
#10482=CARTESIAN_POINT('Ctrl Pts',(-7.53317071863662,-0.229429020332177,
-0.444833694164719));
#10483=CARTESIAN_POINT('Ctrl Pts',(-7.45255927462588,-0.246609536103531,
-0.43960035658631));
#10484=CARTESIAN_POINT('Ctrl Pts',(-7.37194783061514,-0.263790051874886,
-0.434367019007902));
#10485=CARTESIAN_POINT('Ctrl Pts',(-7.28210108896861,-0.237638301729805,
-0.429133681429493));
#10486=CARTESIAN_POINT('Ctrl Pts',(-7.22330226728795,-0.179879548304771,
-0.423900343851085));
#10487=CARTESIAN_POINT('Ctrl Pts',(-7.16450344560729,-0.122120794879737,
-0.418667006272676));
#10488=CARTESIAN_POINT('Ctrl Pts',(-7.13675254389251,-0.0327550381747478,
-0.413433668694268));
#10489=CARTESIAN_POINT('Ctrl Pts',(-7.15249181203852,0.048150156136099,
-0.408200331115859));
#10490=CARTESIAN_POINT('Ctrl Pts',(-7.16823108018453,0.129055350446945,
-0.402966993537451));
#10491=CARTESIAN_POINT('Ctrl Pts',(-7.22746051819134,0.201499982363649,
-0.397733655959043));
#10492=CARTESIAN_POINT('Ctrl Pts',(-7.30362432341862,0.233003153647928,
-0.392500318380634));
#10493=CARTESIAN_POINT('Ctrl Pts',(-7.37978812864591,0.264506324932207,
-0.387266980802226));
#10494=CARTESIAN_POINT('Ctrl Pts',(-7.47288630109367,0.255068035584059,
-0.382033643223817));
#10495=CARTESIAN_POINT('Ctrl Pts',(-7.54117782857522,0.20891998793682,-0.376800305645408));
#10496=CARTESIAN_POINT('Ctrl Pts',(-7.60878192914431,0.163236469508371,
-0.371619647180005));
#10497=CARTESIAN_POINT('Ctrl Pts',(-7.65207628176844,0.0815785187217153,
-0.366438988714602));
#10498=CARTESIAN_POINT('Ctrl Pts',(-7.65214708790382,-1.47686313733716E-5,
-0.361258330249198));
#10499=CARTESIAN_POINT('Origin',(-7.4,0.,-0.45));
#10500=CARTESIAN_POINT('',(-7.65148582098249,0.000162483271353819,-0.261258330249198));
#10501=CARTESIAN_POINT('',(-7.65138929442701,-8.15071719056464E-5,-0.288741669750802));
#10502=CARTESIAN_POINT('',(-7.65175,3.08304831685346E-17,-0.45));
#10503=CARTESIAN_POINT('Ctrl Pts',(-7.65138929442701,-8.15071719056464E-5,
-0.288741669750802));
#10504=CARTESIAN_POINT('Ctrl Pts',(-7.65125007315824,0.0467834313418686,
-0.291694310658131));
#10505=CARTESIAN_POINT('Ctrl Pts',(-7.63865917700223,0.0937178577187305,
-0.29464695156546));
#10506=CARTESIAN_POINT('Ctrl Pts',(-7.61409346854159,0.133201947889911,
-0.297599592472789));
#10507=CARTESIAN_POINT('Ctrl Pts',(-7.57055256761178,0.203184576772822,
-0.302832930051198));
#10508=CARTESIAN_POINT('Ctrl Pts',(-7.48939286562526,0.249762019136108,
-0.308066267629606));
#10509=CARTESIAN_POINT('Ctrl Pts',(-7.40700270411694,0.252051055092709,
-0.313299605208014));
#10510=CARTESIAN_POINT('Ctrl Pts',(-7.32461254260861,0.254340091049311,
-0.318532942786423));
#10511=CARTESIAN_POINT('Ctrl Pts',(-7.2409919215785,0.212340720599228,-0.323766280364831));
#10512=CARTESIAN_POINT('Ctrl Pts',(-7.19363254765278,0.144883563035952,
-0.32899961794324));
#10513=CARTESIAN_POINT('Ctrl Pts',(-7.14627317372706,0.0774264054726766,
-0.334232955521648));
#10514=CARTESIAN_POINT('Ctrl Pts',(-7.13517504690573,-0.0154885392037914,
-0.339466293100057));
#10515=CARTESIAN_POINT('Ctrl Pts',(-7.16531406554617,-0.0922024099003809,
-0.344699630678465));
#10516=CARTESIAN_POINT('Ctrl Pts',(-7.1954530841866,-0.168916280596969,
-0.349932968256874));
#10517=CARTESIAN_POINT('Ctrl Pts',(-7.2668292482888,-0.22942907731368,-0.355166305835282));
#10518=CARTESIAN_POINT('Ctrl Pts',(-7.3474407123204,-0.246609597351995,
-0.36039964341369));
#10519=CARTESIAN_POINT('Ctrl Pts',(-7.42805217635201,-0.263790117390309,
-0.365632980992099));
#10520=CARTESIAN_POINT('Ctrl Pts',(-7.51789894031303,-0.237638360750227,
-0.370866318570507));
#10521=CARTESIAN_POINT('Ctrl Pts',(-7.57669777659709,-0.179879592980104,
-0.376099656148916));
#10522=CARTESIAN_POINT('Ctrl Pts',(-7.6240439603623,-0.133370896452756,
-0.380313660682878));
#10523=CARTESIAN_POINT('Ctrl Pts',(-7.65125915495639,-0.0663687098152037,
-0.38452766521684));
#10524=CARTESIAN_POINT('Ctrl Pts',(-7.65184733409926,0.000207924010478792,
-0.388741669750802));
#10525=CARTESIAN_POINT('Ctrl Pts',(-7.65214708790382,-1.47686313733716E-5,
-0.361258330249198));
#10526=CARTESIAN_POINT('Ctrl Pts',(-7.65214780789037,-0.000844443475530506,
-0.361205651136193));
#10527=CARTESIAN_POINT('Ctrl Pts',(-7.65214405870171,-0.00167411163369731,
-0.361152972023188));
#10528=CARTESIAN_POINT('Ctrl Pts',(-7.65213582045222,-0.00250373521502267,
-0.361100292910183));
#10529=CARTESIAN_POINT('Ctrl Pts',(-7.6513174023323,-0.0849216047732982,
-0.355866955331775));
#10530=CARTESIAN_POINT('Ctrl Pts',(-7.60619568357711,-0.166899537943519,
-0.350633617753367));
#10531=CARTESIAN_POINT('Ctrl Pts',(-7.53700120324214,-0.211682335038927,
-0.345400280174958));
#10532=CARTESIAN_POINT('Ctrl Pts',(-7.46780672290718,-0.256465132134335,
-0.34016694259655));
#10533=CARTESIAN_POINT('Ctrl Pts',(-7.37453948099245,-0.264052793154931,
-0.334933605018141));
#10534=CARTESIAN_POINT('Ctrl Pts',(-7.29901629276741,-0.231043354126343,
-0.329700267439733));
#10535=CARTESIAN_POINT('Ctrl Pts',(-7.22349310454237,-0.198033915097754,
-0.324466929861324));
#10536=CARTESIAN_POINT('Ctrl Pts',(-7.16571397000702,-0.12442737601998,
-0.319233592282916));
#10537=CARTESIAN_POINT('Ctrl Pts',(-7.15158444133632,-0.0432255812782405,
-0.314000254704507));
#10538=CARTESIAN_POINT('Ctrl Pts',(-7.13745491266562,0.0379762134634984,
-0.308766917126099));
#10539=CARTESIAN_POINT('Ctrl Pts',(-7.16697498985957,0.126773263869202,
-0.303533579547691));
#10540=CARTESIAN_POINT('Ctrl Pts',(-7.22690920460173,0.183352985471641,
-0.298300241969282));
#10541=CARTESIAN_POINT('Ctrl Pts',(-7.28684341934389,0.239932707074081,
-0.293066904390874));
#10542=CARTESIAN_POINT('Ctrl Pts',(-7.37719177163426,0.264295099873255,
-0.287833566812465));
#10543=CARTESIAN_POINT('Ctrl Pts',(-7.45744614455411,0.245517170168018,
-0.282600229234057));
#10544=CARTESIAN_POINT('Ctrl Pts',(-7.53770051747395,0.226739240462782,
-0.277366891655648));
#10545=CARTESIAN_POINT('Ctrl Pts',(-7.60786091102327,0.164820988253137,
-0.27213355407724));
#10546=CARTESIAN_POINT('Ctrl Pts',(-7.63647057578236,0.0875237549501118,
-0.266900216498831));
#10547=CARTESIAN_POINT('Ctrl Pts',(-7.64675161675558,0.0597465674368453,
-0.265019587748954));
#10548=CARTESIAN_POINT('Ctrl Pts',(-7.65166694660374,0.029983393820629,
-0.263138958999076));
#10549=CARTESIAN_POINT('Ctrl Pts',(-7.65148582098249,0.000162483271353819,
-0.261258330249198));
#10550=CARTESIAN_POINT('Origin',(-7.4,0.,-0.45));
#10551=CARTESIAN_POINT('',(-7.65166448275063,-0.000213511554003356,-0.161258330249198));
#10552=CARTESIAN_POINT('',(-7.65210261813639,-9.36994259479408E-5,-0.188741669750802));
#10553=CARTESIAN_POINT('',(-7.65175,3.08304831685346E-17,-0.45));
#10554=CARTESIAN_POINT('Ctrl Pts',(-7.65210261813639,-9.36994259479408E-5,
-0.188741669750802));
#10555=CARTESIAN_POINT('Ctrl Pts',(-7.65172967198033,0.0768944675440526,
-0.193627618521014));
#10556=CARTESIAN_POINT('Ctrl Pts',(-7.61382774165573,0.154200818874978,
-0.198513567291225));
#10557=CARTESIAN_POINT('Ctrl Pts',(-7.55255992854019,0.20075915469979,-0.203399516061437));
#10558=CARTESIAN_POINT('Ctrl Pts',(-7.48693600086431,0.250627767720387,
-0.208632853639845));
#10559=CARTESIAN_POINT('Ctrl Pts',(-7.39450546443956,0.265220588730429,
-0.213866191218254));
#10560=CARTESIAN_POINT('Ctrl Pts',(-7.31670998310708,0.23799484419977,-0.219099528796662));
#10561=CARTESIAN_POINT('Ctrl Pts',(-7.2389145017746,0.210769099669111,-0.224332866375071));
#10562=CARTESIAN_POINT('Ctrl Pts',(-7.17575407553438,0.141724789597751,
-0.229566203953479));
#10563=CARTESIAN_POINT('Ctrl Pts',(-7.15554698967948,0.0618182676595837,
-0.234799541531888));
#10564=CARTESIAN_POINT('Ctrl Pts',(-7.13533990382458,-0.0180882542785847,
-0.240032879110296));
#10565=CARTESIAN_POINT('Ctrl Pts',(-7.15808615835499,-0.108856988083561,
-0.245266216688704));
#10566=CARTESIAN_POINT('Ctrl Pts',(-7.21358735835509,-0.169791339561135,
-0.250499554267113));
#10567=CARTESIAN_POINT('Ctrl Pts',(-7.26908855835519,-0.230725691038708,
-0.255732891845522));
#10568=CARTESIAN_POINT('Ctrl Pts',(-7.35734470382498,-0.261825660188879,
-0.26096622942393));
#10569=CARTESIAN_POINT('Ctrl Pts',(-7.43878572988034,-0.249147425173802,
-0.266199567002338));
#10570=CARTESIAN_POINT('Ctrl Pts',(-7.5202267559357,-0.236469190158724,
-0.271432904580747));
#10571=CARTESIAN_POINT('Ctrl Pts',(-7.59485266257662,-0.180012750978398,
-0.276666242159155));
#10572=CARTESIAN_POINT('Ctrl Pts',(-7.62920456596055,-0.105090623686967,
-0.281899579737564));
#10573=CARTESIAN_POINT('Ctrl Pts',(-7.64417517898123,-0.0724394438722447,
-0.284180276408643));
#10574=CARTESIAN_POINT('Ctrl Pts',(-7.65149683255786,-0.0362812052094826,
-0.286460973079722));
#10575=CARTESIAN_POINT('Ctrl Pts',(-7.65138929442701,-8.15071719056464E-5,
-0.288741669750802));
#10576=CARTESIAN_POINT('Ctrl Pts',(-7.65148582098249,0.000162483271353819,
-0.261258330249198));
#10577=CARTESIAN_POINT('Ctrl Pts',(-7.65116291755486,-0.0530010292400235,
-0.257905621420667));
#10578=CARTESIAN_POINT('Ctrl Pts',(-7.63464229858077,-0.106348043093427,
-0.254552912592137));
#10579=CARTESIAN_POINT('Ctrl Pts',(-7.60344957268528,-0.148953054949818,
-0.251200203763606));
#10580=CARTESIAN_POINT('Ctrl Pts',(-7.55475996886024,-0.215456417150318,
-0.245966866185197));
#10581=CARTESIAN_POINT('Ctrl Pts',(-7.47032182524129,-0.255786927154911,
-0.240733528606789));
#10582=CARTESIAN_POINT('Ctrl Pts',(-7.38799338681216,-0.251862223513114,
-0.235500191028381));
#10583=CARTESIAN_POINT('Ctrl Pts',(-7.30566494838303,-0.247937519871316,
-0.230266853449972));
#10584=CARTESIAN_POINT('Ctrl Pts',(-7.22544621514372,-0.199757602583128,
-0.225033515871564));
#10585=CARTESIAN_POINT('Ctrl Pts',(-7.18330364444125,-0.128924136071955,
-0.219800178293155));
#10586=CARTESIAN_POINT('Ctrl Pts',(-7.14116107373879,-0.0580906695607829,
-0.214566840714747));
#10587=CARTESIAN_POINT('Ctrl Pts',(-7.13709466557317,0.0353963461733736,
-0.209333503136338));
#10588=CARTESIAN_POINT('Ctrl Pts',(-7.17292760647834,0.109621493446434,
-0.20410016555793));
#10589=CARTESIAN_POINT('Ctrl Pts',(-7.20876054738351,0.183846640719495,
-0.198866827979521));
#10590=CARTESIAN_POINT('Ctrl Pts',(-7.28449283735947,0.23880991953146,-0.193633490401113));
#10591=CARTESIAN_POINT('Ctrl Pts',(-7.36616955518689,0.249868412754667,
-0.188400152822705));
#10592=CARTESIAN_POINT('Ctrl Pts',(-7.44784627301432,0.260926905977874,
-0.183166815244296));
#10593=CARTESIAN_POINT('Ctrl Pts',(-7.53546741869321,0.228080613612323,
-0.177933477665888));
#10594=CARTESIAN_POINT('Ctrl Pts',(-7.58974760249707,0.166056061051272,
-0.172700140087479));
#10595=CARTESIAN_POINT('Ctrl Pts',(-7.62930575773839,0.120853987162775,
-0.168886203474719));
#10596=CARTESIAN_POINT('Ctrl Pts',(-7.65115599235281,0.0601548704022266,
-0.165072266861958));
#10597=CARTESIAN_POINT('Ctrl Pts',(-7.65166448275063,-0.000213511554003356,
-0.161258330249198));
#10598=CARTESIAN_POINT('Origin',(-7.4,0.,-0.45));
#10599=CARTESIAN_POINT('',(-7.65205352925247,0.000126382978640343,-0.0612583302491982));
#10600=CARTESIAN_POINT('',(-7.65159361924534,0.000201202514259572,-0.0887416697508019));
#10601=CARTESIAN_POINT('',(-7.65175,3.08304831685346E-17,-0.45));
#10602=CARTESIAN_POINT('',(-7.20865340033349,0.163598720337495,0.));
#10603=CARTESIAN_POINT('Ctrl Pts',(-7.65205352925247,0.000126382978640343,
-0.0612583302491982));
#10604=CARTESIAN_POINT('Ctrl Pts',(-7.65157449481833,-0.0742619827859457,
-0.0565388995680243));
#10605=CARTESIAN_POINT('Ctrl Pts',(-7.61652851723279,-0.14902715398977,
-0.0518194688868503));
#10606=CARTESIAN_POINT('Ctrl Pts',(-7.55878735064402,-0.195852509824499,
-0.0471000382056764));
#10607=CARTESIAN_POINT('Ctrl Pts',(-7.49475864944166,-0.247776758927207,
-0.0418667006272679));
#10608=CARTESIAN_POINT('Ctrl Pts',(-7.40282301710629,-0.26534507015853,
-0.0366333630488594));
#10609=CARTESIAN_POINT('Ctrl Pts',(-7.3242152913777,-0.240530493415837,
-0.0314000254704509));
#10610=CARTESIAN_POINT('Ctrl Pts',(-7.24560756564911,-0.215715916673145,
-0.0261666878920424));
#10611=CARTESIAN_POINT('Ctrl Pts',(-7.18032774652728,-0.148518451956437,
-0.020933350313634));
#10612=CARTESIAN_POINT('Ctrl Pts',(-7.15764056021304,-0.0694194541751962,
-0.0157000127352255));
#10613=CARTESIAN_POINT('Ctrl Pts',(-7.1349533738988,0.00967954360604439,
-0.010466675156817));
#10614=CARTESIAN_POINT('Ctrl Pts',(-7.15485882039215,0.100680074451818,
-0.00523333757840849));
#10615=CARTESIAN_POINT('Ctrl Pts',(-7.20865340033349,0.163598720337495,
0.));
#10616=CARTESIAN_POINT('',(-7.59170239456967,0.163827044623994,1.51684295230343E-16));
#10617=CARTESIAN_POINT('Origin',(-7.4,0.,0.));
#10618=CARTESIAN_POINT('Ctrl Pts',(-7.59170406260212,0.163828115050569,
9.71445146547012E-17));
#10619=CARTESIAN_POINT('Ctrl Pts',(-7.54033259098557,0.223538299415699,
-0.00499978774624421));
#10620=CARTESIAN_POINT('Ctrl Pts',(-7.45859288812061,0.257577547385412,
-0.00999957549248855));
#10621=CARTESIAN_POINT('Ctrl Pts',(-7.3800820254476,0.251346298664483,-0.0149993632387328));
#10622=CARTESIAN_POINT('Ctrl Pts',(-7.29790376733084,0.244823976168664,
-0.0202327008171413));
#10623=CARTESIAN_POINT('Ctrl Pts',(-7.21926304559467,0.19418105970145,-0.0254660383955497));
#10624=CARTESIAN_POINT('Ctrl Pts',(-7.17937085476038,0.122067692519252,
-0.0306993759739582));
#10625=CARTESIAN_POINT('Ctrl Pts',(-7.13947866392609,0.0499543253370541,
-0.0359327135523666));
#10626=CARTESIAN_POINT('Ctrl Pts',(-7.13833500399368,-0.0436294925601266,
-0.0411660511307751));
#10627=CARTESIAN_POINT('Ctrl Pts',(-7.17647638632986,-0.116697424671654,
-0.0463993887091836));
#10628=CARTESIAN_POINT('Ctrl Pts',(-7.21461776866604,-0.189765356783182,
-0.051632726287592));
#10629=CARTESIAN_POINT('Ctrl Pts',(-7.29204419327081,-0.242317403109057,
-0.0568660638660004));
#10630=CARTESIAN_POINT('Ctrl Pts',(-7.37402938284013,-0.25080526728572,
-0.0620994014444088));
#10631=CARTESIAN_POINT('Ctrl Pts',(-7.45601457240945,-0.259293131462382,
-0.0673327390228173));
#10632=CARTESIAN_POINT('Ctrl Pts',(-7.54255852694332,-0.223716813489832,
-0.0725660766012258));
#10633=CARTESIAN_POINT('Ctrl Pts',(-7.59486468239543,-0.160020353024002,
-0.0777994141796342));
#10634=CARTESIAN_POINT('Ctrl Pts',(-7.63131989619396,-0.11562657060164,
-0.0814468327033568));
#10635=CARTESIAN_POINT('Ctrl Pts',(-7.65114406502439,-0.0575734009856725,
-0.0850942512270794));
#10636=CARTESIAN_POINT('Ctrl Pts',(-7.65159361924534,0.000201202514259572,
-0.0887416697508019));
#10637=CARTESIAN_POINT('Origin',(0.,7.4,0.220842344717745));
#10638=CARTESIAN_POINT('',(-0.307744900822632,7.40014697529577,-0.720842344717746));
#10639=CARTESIAN_POINT('',(-0.306871987992451,7.39998793159208,-0.729157655282255));
#10640=CARTESIAN_POINT('',(-0.30735,7.40000000000001,0.220842344717745));
#10641=CARTESIAN_POINT('',(0.0793799282532798,7.10307770462543,-0.8));
#10642=CARTESIAN_POINT('Ctrl Pts',(-0.306871987992451,7.39998793159208,
-0.729157655282255));
#10643=CARTESIAN_POINT('Ctrl Pts',(-0.306838385861804,7.45195236281704,
-0.731838419874536));
#10644=CARTESIAN_POINT('Ctrl Pts',(-0.269833682477504,7.60539570033716,
-0.739752522045226));
#10645=CARTESIAN_POINT('Ctrl Pts',(-0.0286357467853838,7.76072171687769,
-0.752899961794324));
#10646=CARTESIAN_POINT('Ctrl Pts',(0.285303569958047,7.62301619686966,-0.76859997452955));
#10647=CARTESIAN_POINT('Ctrl Pts',(0.342929470763259,7.28476159359493,-0.784299987264775));
#10648=CARTESIAN_POINT('Ctrl Pts',(0.177014005842301,7.12917943627315,-0.794766662421592));
#10649=CARTESIAN_POINT('Ctrl Pts',(0.0793799282532802,7.10307770462543,
-0.8));
#10650=CARTESIAN_POINT('',(-0.0795800004915529,7.10260193843563,-0.8));
#10651=CARTESIAN_POINT('Origin',(0.,7.4,-0.8));
#10652=CARTESIAN_POINT('Ctrl Pts',(-0.307744900822632,7.40014697529577,
-0.720842344717746));
#10653=CARTESIAN_POINT('Ctrl Pts',(-0.307796455021018,7.40885909073305,
-0.721295091751952));
#10654=CARTESIAN_POINT('Ctrl Pts',(-0.303543375023605,7.51822382240117,
-0.726981176364568));
#10655=CARTESIAN_POINT('Ctrl Pts',(-0.173198863217152,7.71778292610997,
-0.73790059855559));
#10656=CARTESIAN_POINT('Ctrl Pts',(0.169525116851479,7.71979476003134,-0.753600611290817));
#10657=CARTESIAN_POINT('Ctrl Pts',(0.360224711692468,7.43495575882791,-0.769300624026041));
#10658=CARTESIAN_POINT('Ctrl Pts',(0.229894698648723,7.12364967101413,-0.784767086929103));
#10659=CARTESIAN_POINT('Ctrl Pts',(0.0133964428701133,7.07805035355335,
-0.795000212253756));
#10660=CARTESIAN_POINT('Ctrl Pts',(-0.0795809384672905,7.10259970795555,
-0.8));
#10661=CARTESIAN_POINT('Origin',(0.,7.4,0.220842344717745));
#10662=CARTESIAN_POINT('',(-0.306892537291858,7.40006920001046,-0.620842344717746));
#10663=CARTESIAN_POINT('',(-0.307676148864859,7.39981196746108,-0.629157655282254));
#10664=CARTESIAN_POINT('',(-0.30735,7.40000000000001,0.220842344717745));
#10665=CARTESIAN_POINT('Ctrl Pts',(-0.307676148864859,7.39981196746108,
-0.629157655282254));
#10666=CARTESIAN_POINT('Ctrl Pts',(-0.307031426701065,7.48865284062119,
-0.633771727737418));
#10667=CARTESIAN_POINT('Ctrl Pts',(-0.220226223500933,7.67935845555228,
-0.643619137770991));
#10668=CARTESIAN_POINT('Ctrl Pts',(0.101895231555572,7.74728571705174,-0.658699885382972));
#10669=CARTESIAN_POINT('Ctrl Pts',(0.345877106706635,7.50659191670458,-0.674399898118198));
#10670=CARTESIAN_POINT('Ctrl Pts',(0.279700633697489,7.17030794277179,-0.690099910853422));
#10671=CARTESIAN_POINT('Ctrl Pts',(-0.0372719056216933,7.04000753659561,
-0.705799923588649));
#10672=CARTESIAN_POINT('Ctrl Pts',(-0.27243006304546,7.19961759943849,-0.718819171731592));
#10673=CARTESIAN_POINT('Ctrl Pts',(-0.306903983301257,7.35050838990976,
-0.726605082296127));
#10674=CARTESIAN_POINT('Ctrl Pts',(-0.306871987992451,7.39998793159208,
-0.729157655282255));
#10675=CARTESIAN_POINT('Ctrl Pts',(-0.306892537291858,7.40006920001046,
-0.620842344717746));
#10676=CARTESIAN_POINT('Ctrl Pts',(-0.306987708470476,7.44631180509704,
-0.623228399614835));
#10677=CARTESIAN_POINT('Ctrl Pts',(-0.275630272390186,7.59385583250629,
-0.630847792090333));
#10678=CARTESIAN_POINT('Ctrl Pts',(-0.0485593254958618,7.75865428087583,
-0.643700522144239));
#10679=CARTESIAN_POINT('Ctrl Pts',(0.27235863905538,7.63835266345873,-0.659400534879465));
#10680=CARTESIAN_POINT('Ctrl Pts',(0.349049856868627,7.30431662403272,-0.67510054761469));
#10681=CARTESIAN_POINT('Ctrl Pts',(0.112745006295209,7.05608341261925,-0.690800560349915));
#10682=CARTESIAN_POINT('Ctrl Pts',(-0.214930081152626,7.11450349903993,
-0.706047826050933));
#10683=CARTESIAN_POINT('Ctrl Pts',(-0.307200536100844,7.30815508240031,
-0.716061754173544));
#10684=CARTESIAN_POINT('Ctrl Pts',(-0.307744900822632,7.40014697529577,
-0.720842344717746));
#10685=CARTESIAN_POINT('Origin',(0.,7.4,0.220842344717745));
#10686=CARTESIAN_POINT('',(-0.307527055318605,7.3997579348702,-0.520842344717746));
#10687=CARTESIAN_POINT('',(-0.307303201782415,7.40026451811874,-0.529157655282254));
#10688=CARTESIAN_POINT('',(-0.30735,7.40000000000001,0.220842344717745));
#10689=CARTESIAN_POINT('Ctrl Pts',(-0.307303201782415,7.40026451811874,
-0.529157655282254));
#10690=CARTESIAN_POINT('Ctrl Pts',(-0.307524010692625,7.42564508780896,
-0.530471698021893));
#10691=CARTESIAN_POINT('Ctrl Pts',(-0.293133012622773,7.55186005371301,
-0.537019078339939));
#10692=CARTESIAN_POINT('Ctrl Pts',(-0.119552197626099,7.74161126864207,
-0.548799796236395));
#10693=CARTESIAN_POINT('Ctrl Pts',(0.21898032116491,7.68816416491483,-0.56449980897162));
#10694=CARTESIAN_POINT('Ctrl Pts',(0.361151136941273,7.37631755024098,-0.580199821706846));
#10695=CARTESIAN_POINT('Ctrl Pts',(0.17947415907044,7.08570709394078,-0.59589983444207));
#10696=CARTESIAN_POINT('Ctrl Pts',(-0.163138808425949,7.0769263467909,-0.611599847177296));
#10697=CARTESIAN_POINT('Ctrl Pts',(-0.301766089733603,7.27528825889535,
-0.622685787457357));
#10698=CARTESIAN_POINT('Ctrl Pts',(-0.307762678487899,7.38788843249251,
-0.62853839015901));
#10699=CARTESIAN_POINT('Ctrl Pts',(-0.307676148864859,7.39981196746108,
-0.629157655282254));
#10700=CARTESIAN_POINT('Ctrl Pts',(-0.307527055318605,7.3997579348702,-0.520842344717746));
#10701=CARTESIAN_POINT('Ctrl Pts',(-0.306808481761244,7.48302961068977,
-0.525161707477718));
#10702=CARTESIAN_POINT('Ctrl Pts',(-0.229186183907421,7.66837439690706,
-0.534714407816098));
#10703=CARTESIAN_POINT('Ctrl Pts',(0.0824566524067525,7.75240874841395,
-0.549500445732887));
#10704=CARTESIAN_POINT('Ctrl Pts',(0.339423512150486,7.52562925031437,-0.565200458468112));
#10705=CARTESIAN_POINT('Ctrl Pts',(0.292026050158285,7.1861967789166,-0.580900471203337));
#10706=CARTESIAN_POINT('Ctrl Pts',(-0.0172339683272763,7.03848374595487,
-0.596600483938563));
#10707=CARTESIAN_POINT('Ctrl Pts',(-0.26638808838325,7.18812740699665,-0.609914441776699));
#10708=CARTESIAN_POINT('Ctrl Pts',(-0.30677896938989,7.34488783399801,-0.617995062036427));
#10709=CARTESIAN_POINT('Ctrl Pts',(-0.306892537291858,7.40006920001046,
-0.620842344717746));
#10710=CARTESIAN_POINT('Origin',(0.,7.4,0.220842344717745));
#10711=CARTESIAN_POINT('',(-0.307468830726541,7.40025384486444,-0.420842344717745));
#10712=CARTESIAN_POINT('',(-0.306988859154633,7.39982445436712,-0.429157655282254));
#10713=CARTESIAN_POINT('',(-0.30735,7.40000000000001,0.220842344717745));
#10714=CARTESIAN_POINT('Ctrl Pts',(-0.306988859154633,7.39982445436712,
-0.429157655282254));
#10715=CARTESIAN_POINT('Ctrl Pts',(-0.306653737582139,7.462709657289,-0.432405005884775));
#10716=CARTESIAN_POINT('Ctrl Pts',(-0.257472827761211,7.62742015105949,
-0.440885694065705));
#10717=CARTESIAN_POINT('Ctrl Pts',(0.0100514892332193,7.76178716191776,
-0.454599719825043));
#10718=CARTESIAN_POINT('Ctrl Pts',(0.307303884459003,7.59119441739787,-0.470299732560268));
#10719=CARTESIAN_POINT('Ctrl Pts',(0.328993939119635,7.24915580545685,-0.485999745295493));
#10720=CARTESIAN_POINT('Ctrl Pts',(0.0556719707952805,7.04238062809055,
-0.501699758030718));
#10721=CARTESIAN_POINT('Ctrl Pts',(-0.240517094087265,7.14675263225517,
-0.516085728026306));
#10722=CARTESIAN_POINT('Ctrl Pts',(-0.30664461192378,7.32456383290414,-0.525238360443484));
#10723=CARTESIAN_POINT('Ctrl Pts',(-0.307303201782415,7.40026451811874,
-0.529157655282254));
#10724=CARTESIAN_POINT('Ctrl Pts',(-0.307468830726541,7.40025384486444,
-0.420842344717745));
#10725=CARTESIAN_POINT('Ctrl Pts',(-0.307642528584636,7.41991489343264,
-0.421861677762192));
#10726=CARTESIAN_POINT('Ctrl Pts',(-0.297040503111005,7.54033087178353,
-0.428114348385046));
#10727=CARTESIAN_POINT('Ctrl Pts',(-0.138335057048331,7.73444646717113,
-0.43960035658631));
#10728=CARTESIAN_POINT('Ctrl Pts',(0.202642862416027,7.69987813805627,-0.455300369321535));
#10729=CARTESIAN_POINT('Ctrl Pts',(0.361908983097054,7.39640620579093,-0.47100038205676));
#10730=CARTESIAN_POINT('Ctrl Pts',(0.196647846607491,7.09615686298222,-0.486700394791986));
#10731=CARTESIAN_POINT('Ctrl Pts',(-0.144949300426615,7.06836657665492,
-0.502400407527211));
#10732=CARTESIAN_POINT('Ctrl Pts',(-0.298348535773798,7.26378637486166,
-0.513781057502464));
#10733=CARTESIAN_POINT('Ctrl Pts',(-0.307679105093796,7.38213769340927,
-0.519928369899309));
#10734=CARTESIAN_POINT('Ctrl Pts',(-0.307527055318605,7.3997579348702,-0.520842344717746));
#10735=CARTESIAN_POINT('Origin',(0.,7.4,0.220842344717745));
#10736=CARTESIAN_POINT('',(-0.306909631150515,7.39990049164138,-0.320842344717745));
#10737=CARTESIAN_POINT('',(-0.307834810501565,7.3999819696555,-0.329157655282254));
#10738=CARTESIAN_POINT('',(-0.30735,7.40000000000001,0.220842344717745));
#10739=CARTESIAN_POINT('Ctrl Pts',(-0.307834810501565,7.3999819696555,-0.329157655282254));
#10740=CARTESIAN_POINT('Ctrl Pts',(-0.307748366539647,7.49959547048682,
-0.334338313747658));
#10741=CARTESIAN_POINT('Ctrl Pts',(-0.201498726273864,7.69999407607993,
-0.34475230979147));
#10742=CARTESIAN_POINT('Ctrl Pts',(0.138335033537924,7.73444641033119,-0.36039964341369));
#10743=CARTESIAN_POINT('Ctrl Pts',(0.355266543354486,7.46911342881649,-0.376099656148916));
#10744=CARTESIAN_POINT('Ctrl Pts',(0.25362713547982,7.1418057726863,-0.391799668884141));
#10745=CARTESIAN_POINT('Ctrl Pts',(-0.0754421579893288,7.0460233571473,
-0.407499681619367));
#10746=CARTESIAN_POINT('Ctrl Pts',(-0.282790383856574,7.22181342935611,
-0.419952343752071));
#10747=CARTESIAN_POINT('Ctrl Pts',(-0.307193809946764,7.36136565848536,
-0.427171668306367));
#10748=CARTESIAN_POINT('Ctrl Pts',(-0.306988859154633,7.39982445436712,
-0.429157655282254));
#10749=CARTESIAN_POINT('Ctrl Pts',(-0.306909631150515,7.39990049164138,
-0.320842344717745));
#10750=CARTESIAN_POINT('Ctrl Pts',(-0.306739662304611,7.45711574030953,
-0.323794985625074));
#10751=CARTESIAN_POINT('Ctrl Pts',(-0.264122910345685,7.61597598206296,
-0.331980964110812));
#10752=CARTESIAN_POINT('Ctrl Pts',(-0.0100514909408711,7.76178722340353,
-0.345400280174958));
#10753=CARTESIAN_POINT('Ctrl Pts',(0.296214223541038,7.60796192241644,-0.361100292910183));
#10754=CARTESIAN_POINT('Ctrl Pts',(0.336861801835373,7.26765517072256,-0.376800305645408));
#10755=CARTESIAN_POINT('Ctrl Pts',(0.0754421708108413,7.04602329698811,
-0.392500318380633));
#10756=CARTESIAN_POINT('Ctrl Pts',(-0.232262147395604,7.13558699513454,
-0.407180998071413));
#10757=CARTESIAN_POINT('Ctrl Pts',(-0.30675074985441,7.31897349369731,-0.416628340183783));
#10758=CARTESIAN_POINT('Ctrl Pts',(-0.307468830726541,7.40025384486444,
-0.420842344717745));
#10759=CARTESIAN_POINT('Origin',(0.,7.4,0.220842344717745));
#10760=CARTESIAN_POINT('',(-0.307780495269994,7.39988560667899,-0.220842344717745));
#10761=CARTESIAN_POINT('',(-0.307027500057518,7.40019836837334,-0.229157655282254));
#10762=CARTESIAN_POINT('',(-0.30735,7.40000000000001,0.220842344717745));
#10763=CARTESIAN_POINT('Ctrl Pts',(-0.307027500057518,7.40019836837334,
-0.229157655282254));
#10764=CARTESIAN_POINT('Ctrl Pts',(-0.307248628018252,7.43660534980473,
-0.231038284032132));
#10765=CARTESIAN_POINT('Ctrl Pts',(-0.284548663759526,7.57405756525429,
-0.238152250360418));
#10766=CARTESIAN_POINT('Ctrl Pts',(-0.0824566383942325,7.75240868850505,
-0.250499554267113));
#10767=CARTESIAN_POINT('Ctrl Pts',(0.248449835333973,7.66317990580525,-0.266199567002338));
#10768=CARTESIAN_POINT('Ctrl Pts',(0.356568958714344,7.3379551719626,-0.281899579737564));
#10769=CARTESIAN_POINT('Ctrl Pts',(0.144949275792185,7.0683666330192,-0.297599592472788));
#10770=CARTESIAN_POINT('Ctrl Pts',(-0.196647813186698,7.09615691462004,
-0.313299605208015));
#10771=CARTESIAN_POINT('Ctrl Pts',(-0.30737639510771,7.29733055204229,-0.323818959477836));
#10772=CARTESIAN_POINT('Ctrl Pts',(-0.307835689500107,7.39896905770576,
-0.329104976169249));
#10773=CARTESIAN_POINT('Ctrl Pts',(-0.307834810501565,7.3999819696555,-0.329157655282254));
#10774=CARTESIAN_POINT('Ctrl Pts',(-0.307780495269994,7.39988560667899,
-0.220842344717745));
#10775=CARTESIAN_POINT('Ctrl Pts',(-0.307325182455431,7.49387691995895,
-0.225728293487957));
#10776=CARTESIAN_POINT('Ctrl Pts',(-0.211489763984475,7.68934681995645,
-0.235847579836577));
#10777=CARTESIAN_POINT('Ctrl Pts',(0.119552217972776,7.7416113266484,-0.251200203763606));
#10778=CARTESIAN_POINT('Ctrl Pts',(0.350881199163606,7.48873225573956,-0.266900216498831));
#10779=CARTESIAN_POINT('Ctrl Pts',(0.267571630187383,7.15628613456826,-0.282600229234056));
#10780=CARTESIAN_POINT('Ctrl Pts',(-0.0556719802611724,7.04238056731933,
-0.298300241969282));
#10781=CARTESIAN_POINT('Ctrl Pts',(-0.277591376746854,7.21026836224977,
-0.311047613797178));
#10782=CARTESIAN_POINT('Ctrl Pts',(-0.307040919510058,7.35570594470255,
-0.318561648046666));
#10783=CARTESIAN_POINT('Ctrl Pts',(-0.306909631150515,7.39990049164138,
-0.320842344717745));
#10784=CARTESIAN_POINT('Origin',(0.,7.4,0.220842344717745));
#10785=CARTESIAN_POINT('',(-0.307159081926734,7.40024563889874,-0.120842344717745));
#10786=CARTESIAN_POINT('',(-0.307245619935592,7.39973933390828,-0.129157655282254));
#10787=CARTESIAN_POINT('',(-0.30735,7.40000000000001,0.220842344717745));
#10788=CARTESIAN_POINT('Ctrl Pts',(-0.307245619935592,7.39973933390828,
-0.129157655282254));
#10789=CARTESIAN_POINT('Ctrl Pts',(-0.306624827350326,7.47344032150659,
-0.132971591895015));
#10790=CARTESIAN_POINT('Ctrl Pts',(-0.243345164403822,7.64922880659321,
-0.142018866086184));
#10791=CARTESIAN_POINT('Ctrl Pts',(0.0485593171240025,7.7586542191763,-0.156299477855761));
#10792=CARTESIAN_POINT('Ctrl Pts',(0.325933551193656,7.55734778288709,-0.171999490590986));
#10793=CARTESIAN_POINT('Ctrl Pts',(0.311040077773849,7.21494575887322,-0.187699503326212));
#10794=CARTESIAN_POINT('Ctrl Pts',(0.0172339654105937,7.03848380750682,
-0.203399516061437));
#10795=CARTESIAN_POINT('Ctrl Pts',(-0.254981241847562,7.16850298693634,
-0.217218900046784));
#10796=CARTESIAN_POINT('Ctrl Pts',(-0.306633282077901,7.33529347522358,
-0.225804946453723));
#10797=CARTESIAN_POINT('Ctrl Pts',(-0.307027500057518,7.40019836837334,
-0.229157655282254));
#10798=CARTESIAN_POINT('Ctrl Pts',(-0.307159081926734,7.40024563889874,
-0.120842344717745));
#10799=CARTESIAN_POINT('Ctrl Pts',(-0.307397720825203,7.43091439273595,
-0.122428263772431));
#10800=CARTESIAN_POINT('Ctrl Pts',(-0.28919541585723,7.56250979326726,-0.129247520405525));
#10801=CARTESIAN_POINT('Ctrl Pts',(-0.101895250628719,7.74728578061798,
-0.141300114617028));
#10802=CARTESIAN_POINT('Ctrl Pts',(0.233453631148172,7.67656918324398,-0.157000127352253));
#10803=CARTESIAN_POINT('Ctrl Pts',(0.359464126606772,7.35784834370038,-0.172700140087479));
#10804=CARTESIAN_POINT('Ctrl Pts',(0.163138836475842,7.07692629120202,-0.188400152822704));
#10805=CARTESIAN_POINT('Ctrl Pts',(-0.179474189751402,7.08570704088486,
-0.20410016555793));
#10806=CARTESIAN_POINT('Ctrl Pts',(-0.304612100383046,7.28587761682761,
-0.214914229522943));
#10807=CARTESIAN_POINT('Ctrl Pts',(-0.307812867810814,7.39320286565227,
-0.220494955909548));
#10808=CARTESIAN_POINT('Ctrl Pts',(-0.307780495269994,7.39988560667899,
-0.220842344717745));
#10809=CARTESIAN_POINT('Origin',(0.,7.4,0.220842344717745));
#10810=CARTESIAN_POINT('',(-0.30701976654778,7.39969382919393,-0.0208423447177451));
#10811=CARTESIAN_POINT('',(-0.307720586104713,7.40015430359934,-0.0291576552822542));
#10812=CARTESIAN_POINT('',(-0.30735,7.40000000000001,0.220842344717745));
#10813=CARTESIAN_POINT('',(-0.0793799282532889,7.10307770462543,0.));
#10814=CARTESIAN_POINT('Ctrl Pts',(-0.0793799282532879,7.10307770462543,
5.55111512312578E-17));
#10815=CARTESIAN_POINT('Ctrl Pts',(-0.177014005842308,7.12917943627315,
-0.00523333757840839));
#10816=CARTESIAN_POINT('Ctrl Pts',(-0.287143377782575,7.23245041729098,
-0.0121807858176568));
#10817=CARTESIAN_POINT('Ctrl Pts',(-0.307246205355195,7.36652716202022,
-0.0191282340569052));
#10818=CARTESIAN_POINT('Ctrl Pts',(-0.30701976654778,7.39969382919393,-0.0208423447177451));
#10819=CARTESIAN_POINT('',(0.0795799507667233,7.10260193953608,6.20619955657751E-17));
#10820=CARTESIAN_POINT('Origin',(0.,7.4,0.));
#10821=CARTESIAN_POINT('Ctrl Pts',(0.0795808873001328,7.10259971193733,
-3.33392168039293E-18));
#10822=CARTESIAN_POINT('Ctrl Pts',(-0.0133965346091573,7.07805031897846,
-0.00499978774624427));
#10823=CARTESIAN_POINT('Ctrl Pts',(-0.219022047825184,7.12135984424409,
-0.0147190061736623));
#10824=CARTESIAN_POINT('Ctrl Pts',(-0.307135762589409,7.30933695078315,
-0.0244382246010804));
#10825=CARTESIAN_POINT('Ctrl Pts',(-0.307720586104713,7.40015430359934,
-0.0291576552822542));
#10826=CARTESIAN_POINT('Origin',(7.4,0.,0.220842344717745));
#10827=CARTESIAN_POINT('',(7.09225513659108,0.000146978884224908,-0.720842344717746));
#10828=CARTESIAN_POINT('',(7.0931279909255,-1.20749723882283E-5,-0.729157655282255));
#10829=CARTESIAN_POINT('',(7.09265,5.61065397787037E-15,0.220842344717745));
#10830=CARTESIAN_POINT('',(7.47937992825329,-0.29692229537457,-0.8));
#10831=CARTESIAN_POINT('Ctrl Pts',(7.0931279909255,-1.20749723881847E-5,
-0.729157655282255));
#10832=CARTESIAN_POINT('Ctrl Pts',(7.09316159233691,0.0519523551408496,
-0.731838419874536));
#10833=CARTESIAN_POINT('Ctrl Pts',(7.13016629582236,0.205395693670095,-0.739752522045226));
#10834=CARTESIAN_POINT('Ctrl Pts',(7.37136424992534,0.360721809373367,-0.752899961794324));
#10835=CARTESIAN_POINT('Ctrl Pts',(7.68530360759964,0.223016092822843,-0.768599974529549));
#10836=CARTESIAN_POINT('Ctrl Pts',(7.74292942723977,-0.115238123859802,
-0.784299987264775));
#10837=CARTESIAN_POINT('Ctrl Pts',(7.57701400584231,-0.270820563726849,
-0.794766662421592));
#10838=CARTESIAN_POINT('Ctrl Pts',(7.47937992825329,-0.29692229537457,-0.8));
#10839=CARTESIAN_POINT('',(7.32042003604622,-0.297398060701823,-0.799999999999999));
#10840=CARTESIAN_POINT('Origin',(7.4,0.,-0.8));
#10841=CARTESIAN_POINT('Ctrl Pts',(7.09225513659108,0.000146978884224968,
-0.720842344717746));
#10842=CARTESIAN_POINT('Ctrl Pts',(7.09220358244584,0.00885909314624902,
-0.721295091751953));
#10843=CARTESIAN_POINT('Ctrl Pts',(7.09645666272727,0.118223809389764,-0.726981176364568));
#10844=CARTESIAN_POINT('Ctrl Pts',(7.22680116614257,0.317782866086405,-0.737900598555591));
#10845=CARTESIAN_POINT('Ctrl Pts',(7.56952507950631,0.319794755380677,-0.753600611290817));
#10846=CARTESIAN_POINT('Ctrl Pts',(7.76022470046591,0.0349556943853752,
-0.769300624026041));
#10847=CARTESIAN_POINT('Ctrl Pts',(7.62989460038476,-0.276350197541752,
-0.784767086929103));
#10848=CARTESIAN_POINT('Ctrl Pts',(7.41339651031425,-0.321949671834906,
-0.795000212253756));
#10849=CARTESIAN_POINT('Ctrl Pts',(7.32041909912987,-0.297400289065614,
-0.8));
#10850=CARTESIAN_POINT('Origin',(7.4,0.,0.220842344717745));
#10851=CARTESIAN_POINT('',(7.09310750107417,6.92000663027048E-5,-0.620842344717746));
#10852=CARTESIAN_POINT('',(7.09232382992685,-0.000188032469277442,-0.629157655282255));
#10853=CARTESIAN_POINT('',(7.09265,5.61065397787037E-15,0.220842344717745));
#10854=CARTESIAN_POINT('Ctrl Pts',(7.09232382992685,-0.000188032469277427,
-0.629157655282255));
#10855=CARTESIAN_POINT('Ctrl Pts',(7.09296855206387,0.088652846655831,-0.633771727737419));
#10856=CARTESIAN_POINT('Ctrl Pts',(7.17977376091732,0.279358473971188,-0.643619137770991));
#10857=CARTESIAN_POINT('Ctrl Pts',(7.50189523930833,0.347285742890038,-0.658699885382972));
#10858=CARTESIAN_POINT('Ctrl Pts',(7.74587712940208,0.10659192062098,-0.674399898118197));
#10859=CARTESIAN_POINT('Ctrl Pts',(7.67970065492672,-0.229692066723022,
-0.690099910853423));
#10860=CARTESIAN_POINT('Ctrl Pts',(7.36272808895739,-0.359992499947249,
-0.705799923588647));
#10861=CARTESIAN_POINT('Ctrl Pts',(7.1275699207301,-0.200382398818872,-0.718819171731592));
#10862=CARTESIAN_POINT('Ctrl Pts',(7.09309599630155,-0.0494916155961562,
-0.726605082296128));
#10863=CARTESIAN_POINT('Ctrl Pts',(7.0931279909255,-1.20749723881847E-5,
-0.729157655282255));
#10864=CARTESIAN_POINT('Ctrl Pts',(7.09310750107417,6.92000663027083E-5,
-0.620842344717746));
#10865=CARTESIAN_POINT('Ctrl Pts',(7.09301232990392,0.0463117993985499,
-0.623228399614835));
#10866=CARTESIAN_POINT('Ctrl Pts',(7.12436976205869,0.193855808404846,-0.630847792090333));
#10867=CARTESIAN_POINT('Ctrl Pts',(7.35144068066377,0.358654235479558,-0.643700522144239));
#10868=CARTESIAN_POINT('Ctrl Pts',(7.67235860481237,0.238352634675404,-0.659400534879465));
#10869=CARTESIAN_POINT('Ctrl Pts',(7.74904981361332,-0.0956833658965494,
-0.675100547614689));
#10870=CARTESIAN_POINT('Ctrl Pts',(7.51274499136877,-0.343916540891515,
-0.690800560349916));
#10871=CARTESIAN_POINT('Ctrl Pts',(7.18506994739396,-0.285496471322637,
-0.706047826050933));
#10872=CARTESIAN_POINT('Ctrl Pts',(7.09279950075169,-0.0918449016015606,
-0.716061754173544));
#10873=CARTESIAN_POINT('Ctrl Pts',(7.09225513659108,0.000146978884224968,
-0.720842344717746));
#10874=CARTESIAN_POINT('Origin',(7.4,0.,0.220842344717745));
#10875=CARTESIAN_POINT('',(7.09247298313668,-0.000242065099788365,-0.520842344717745));
#10876=CARTESIAN_POINT('',(7.09269677699397,0.000264518140442497,-0.529157655282254));
#10877=CARTESIAN_POINT('',(7.09265,5.61065397787037E-15,0.220842344717745));
#10878=CARTESIAN_POINT('Ctrl Pts',(7.09269677699397,0.000264518140442521,
-0.529157655282254));
#10879=CARTESIAN_POINT('Ctrl Pts',(7.09247596806863,0.0256450895838866,
-0.530471698021893));
#10880=CARTESIAN_POINT('Ctrl Pts',(7.10686696713217,0.151860064204999,-0.537019078339939));
#10881=CARTESIAN_POINT('Ctrl Pts',(7.28044779410479,0.341611292216308,-0.548799796236394));
#10882=CARTESIAN_POINT('Ctrl Pts',(7.61898033631151,0.288164184858654,-0.564499808971621));
#10883=CARTESIAN_POINT('Ctrl Pts',(7.76115116184634,-0.0236824514715945,
-0.580199821706845));
#10884=CARTESIAN_POINT('Ctrl Pts',(7.57947417153963,-0.314292927621228,
-0.595899834442071));
#10885=CARTESIAN_POINT('Ctrl Pts',(7.23686118017403,-0.323073675801685,
-0.611599847177295));
#10886=CARTESIAN_POINT('Ctrl Pts',(7.09823388955116,-0.12471174942936,-0.622685787457357));
#10887=CARTESIAN_POINT('Ctrl Pts',(7.0922373003074,-0.0121115682384182,
-0.62853839015901));
#10888=CARTESIAN_POINT('Ctrl Pts',(7.09232382992685,-0.000188032469277427,
-0.629157655282255));
#10889=CARTESIAN_POINT('Ctrl Pts',(7.09247298313668,-0.000242065099788339,
-0.520842344717745));
#10890=CARTESIAN_POINT('Ctrl Pts',(7.09319155660411,0.0830296003080465,
-0.525161707477718));
#10891=CARTESIAN_POINT('Ctrl Pts',(7.17081384475125,0.268374363352796,-0.534714407816098));
#10892=CARTESIAN_POINT('Ctrl Pts',(7.4824566420967,0.352408704334569,-0.549500445732887));
#10893=CARTESIAN_POINT('Ctrl Pts',(7.73942346970471,0.125629234627381,-0.565200458468113));
#10894=CARTESIAN_POINT('Ctrl Pts',(7.69202601364555,-0.213803194390989,
-0.580900471203338));
#10895=CARTESIAN_POINT('Ctrl Pts',(7.38276603381877,-0.361516208756931,
-0.596600483938563));
#10896=CARTESIAN_POINT('Ctrl Pts',(7.13361194494272,-0.211872566628196,
-0.609914441776699));
#10897=CARTESIAN_POINT('Ctrl Pts',(7.09322106896615,-0.0551121590794967,
-0.617995062036427));
#10898=CARTESIAN_POINT('Ctrl Pts',(7.09310750107417,6.92000663027083E-5,
-0.620842344717746));
#10899=CARTESIAN_POINT('Origin',(7.4,0.,0.220842344717745));
#10900=CARTESIAN_POINT('',(7.09253120772146,0.000253844832670602,-0.420842344717745));
#10901=CARTESIAN_POINT('',(7.09301111964154,-0.000175545644984122,-0.429157655282254));
#10902=CARTESIAN_POINT('',(7.09265,5.61065397787037E-15,0.220842344717745));
#10903=CARTESIAN_POINT('Ctrl Pts',(7.09301111964154,-0.000175545644984097,
-0.429157655282254));
#10904=CARTESIAN_POINT('Ctrl Pts',(7.0933462412372,0.0627096616204277,-0.432405005884775));
#10905=CARTESIAN_POINT('Ctrl Pts',(7.14252715445512,0.227420166767621,-0.440885694065704));
#10906=CARTESIAN_POINT('Ctrl Pts',(7.41005148992723,0.36178718690615,-0.454599719825043));
#10907=CARTESIAN_POINT('Ctrl Pts',(7.70730390568508,0.191194430604527,-0.470299732560268));
#10908=CARTESIAN_POINT('Ctrl Pts',(7.72899396184246,-0.150844204963527,
-0.485999745295493));
#10909=CARTESIAN_POINT('Ctrl Pts',(7.45567197464232,-0.357619396607422,
-0.501699758030719));
#10910=CARTESIAN_POINT('Ctrl Pts',(7.15948288929725,-0.253247385241686,
-0.516085728026305));
#10911=CARTESIAN_POINT('Ctrl Pts',(7.09335536689775,-0.0754361723033938,
-0.525238360443484));
#10912=CARTESIAN_POINT('Ctrl Pts',(7.09269677699397,0.000264518140442521,
-0.529157655282254));
#10913=CARTESIAN_POINT('Ctrl Pts',(7.09253120772146,0.000253844832670647,
-0.420842344717745));
#10914=CARTESIAN_POINT('Ctrl Pts',(7.09235750988509,0.019914890942319,-0.421861677762192));
#10915=CARTESIAN_POINT('Ctrl Pts',(7.10295953403298,0.140330854235573,-0.428114348385046));
#10916=CARTESIAN_POINT('Ctrl Pts',(7.26166496025002,0.334446425349789,-0.43960035658631));
#10917=CARTESIAN_POINT('Ctrl Pts',(7.60264283707619,0.299878100557217,-0.455300369321535));
#10918=CARTESIAN_POINT('Ctrl Pts',(7.76190893784147,-0.00359379375923244,
-0.47100038205676));
#10919=CARTESIAN_POINT('Ctrl Pts',(7.59664782201734,-0.303843099024022,
-0.486700394791986));
#10920=CARTESIAN_POINT('Ctrl Pts',(7.25505071769875,-0.33163338187372,-0.502400407527211));
#10921=CARTESIAN_POINT('Ctrl Pts',(7.10165150153385,-0.136213608107123,
-0.513781057502464));
#10922=CARTESIAN_POINT('Ctrl Pts',(7.09232093338052,-0.0178623043576069,
-0.519928369899309));
#10923=CARTESIAN_POINT('Ctrl Pts',(7.09247298313668,-0.000242065099788339,
-0.520842344717745));
#10924=CARTESIAN_POINT('Origin',(7.4,0.,0.220842344717745));
#10925=CARTESIAN_POINT('',(7.09309040722717,-9.95083455336276E-5,-0.320842344717745));
#10926=CARTESIAN_POINT('',(7.09216516823616,-1.80303458139274E-5,-0.329157655282254));
#10927=CARTESIAN_POINT('',(7.09265,5.61065397787037E-15,0.220842344717745));
#10928=CARTESIAN_POINT('Ctrl Pts',(7.09216516823616,-1.80303458139253E-5,
-0.329157655282254));
#10929=CARTESIAN_POINT('Ctrl Pts',(7.09225161220405,0.0995954773657983,
-0.334338313747658));
#10930=CARTESIAN_POINT('Ctrl Pts',(7.19850125980854,0.299994096800775,-0.34475230979147));
#10931=CARTESIAN_POINT('Ctrl Pts',(7.53833504309277,0.334446433431464,-0.36039964341369));
#10932=CARTESIAN_POINT('Ctrl Pts',(7.75526656789289,0.0691134335902364,
-0.376099656148916));
#10933=CARTESIAN_POINT('Ctrl Pts',(7.65362715299794,-0.25819424514732,-0.391799668884141));
#10934=CARTESIAN_POINT('Ctrl Pts',(7.32455783679988,-0.353976667301946,
-0.407499681619366));
#10935=CARTESIAN_POINT('Ctrl Pts',(7.11720959661094,-0.178186582951383,
-0.419952343752071));
#10936=CARTESIAN_POINT('Ctrl Pts',(7.09280616883524,-0.0386343441831341,
-0.427171668306367));
#10937=CARTESIAN_POINT('Ctrl Pts',(7.09301111964154,-0.000175545644984097,
-0.429157655282254));
#10938=CARTESIAN_POINT('Ctrl Pts',(7.09309040722717,-9.95083455336103E-5,
-0.320842344717745));
#10939=CARTESIAN_POINT('Ctrl Pts',(7.09326037605201,0.0571157331677331,
-0.323794985625074));
#10940=CARTESIAN_POINT('Ctrl Pts',(7.13587712268272,0.215975955054746,-0.331980964110812));
#10941=CARTESIAN_POINT('Ctrl Pts',(7.38994851031558,0.361787178163918,-0.345400280174957));
#10942=CARTESIAN_POINT('Ctrl Pts',(7.69621418650062,0.207961896411083,-0.361100292910183));
#10943=CARTESIAN_POINT('Ctrl Pts',(7.73686175971175,-0.132344812727946,
-0.376800305645408));
#10944=CARTESIAN_POINT('Ctrl Pts',(7.47544216137711,-0.353976658748332,
-0.392500318380634));
#10945=CARTESIAN_POINT('Ctrl Pts',(7.16773788164802,-0.264412971801384,
-0.407180998071412));
#10946=CARTESIAN_POINT('Ctrl Pts',(7.09324928850379,-0.0810264961705937,
-0.416628340183783));
#10947=CARTESIAN_POINT('Ctrl Pts',(7.09253120772146,0.000253844832670647,
-0.420842344717745));
#10948=CARTESIAN_POINT('Origin',(7.4,0.,0.220842344717745));
#10949=CARTESIAN_POINT('',(7.0922195431951,-0.00011439326538178,-0.220842344717745));
#10950=CARTESIAN_POINT('',(7.09297247873625,0.000198368389210363,-0.229157655282254));
#10951=CARTESIAN_POINT('',(7.09265,5.61065397787037E-15,0.220842344717745));
#10952=CARTESIAN_POINT('Ctrl Pts',(7.09297247873625,0.000198368389210352,
-0.229157655282254));
#10953=CARTESIAN_POINT('Ctrl Pts',(7.09275135076004,0.0366053523330718,
-0.231038284032132));
#10954=CARTESIAN_POINT('Ctrl Pts',(7.11545131658584,0.174057577268075,-0.238152250360418));
#10955=CARTESIAN_POINT('Ctrl Pts',(7.31754335591095,0.352408712852604,-0.250499554267113));
#10956=CARTESIAN_POINT('Ctrl Pts',(7.64844985249427,0.263179923979787,-0.266199567002338));
#10957=CARTESIAN_POINT('Ctrl Pts',(7.75656898334281,-0.062044832321089,
-0.281899579737564));
#10958=CARTESIAN_POINT('Ctrl Pts',(7.54494928580385,-0.331633389887768,
-0.297599592472789));
#10959=CARTESIAN_POINT('Ctrl Pts',(7.20335217323078,-0.303843106366043,
-0.313299605208014));
#10960=CARTESIAN_POINT('Ctrl Pts',(7.09262358366168,-0.102669455049145,
-0.323818959477836));
#10961=CARTESIAN_POINT('Ctrl Pts',(7.09216428923756,-0.00103094236550998,
-0.329104976169249));
#10962=CARTESIAN_POINT('Ctrl Pts',(7.09216516823616,-1.80303458139253E-5,
-0.329157655282254));
#10963=CARTESIAN_POINT('Ctrl Pts',(7.0922195431951,-0.000114393265381769,
-0.220842344717745));
#10964=CARTESIAN_POINT('Ctrl Pts',(7.09267485594448,0.0938769082790096,
-0.225728293487957));
#10965=CARTESIAN_POINT('Ctrl Pts',(7.1885102624992,0.28934678370451,-0.235847579836577));
#10966=CARTESIAN_POINT('Ctrl Pts',(7.51955220300225,0.341611283968803,-0.251200203763605));
#10967=CARTESIAN_POINT('Ctrl Pts',(7.7508811552982,0.0887322446241938,-0.266900216498831));
#10968=CARTESIAN_POINT('Ctrl Pts',(7.66757159672246,-0.243713834945875,
-0.282600229234056));
#10969=CARTESIAN_POINT('Ctrl Pts',(7.34432802670357,-0.357619387966788,
-0.298300241969282));
#10970=CARTESIAN_POINT('Ctrl Pts',(7.12240865796432,-0.189731614023667,
-0.311047613797178));
#10971=CARTESIAN_POINT('Ctrl Pts',(7.0929591188839,-0.044294049757736,-0.318561648046666));
#10972=CARTESIAN_POINT('Ctrl Pts',(7.09309040722717,-9.95083455336103E-5,
-0.320842344717745));
#10973=CARTESIAN_POINT('Origin',(7.4,0.,0.220842344717745));
#10974=CARTESIAN_POINT('',(7.09284095646985,0.00024563841227826,-0.120842344717745));
#10975=CARTESIAN_POINT('',(7.09275435891078,-0.00026066578654145,-0.129157655282254));
#10976=CARTESIAN_POINT('',(7.09265,5.61065397787037E-15,0.220842344717745));
#10977=CARTESIAN_POINT('Ctrl Pts',(7.09275435891078,-0.000260665786541426,
-0.129157655282254));
#10978=CARTESIAN_POINT('Ctrl Pts',(7.09337515152961,0.0734403268284316,
-0.132971591895015));
#10979=CARTESIAN_POINT('Ctrl Pts',(7.15665481869895,0.249228823319743,-0.142018866086184));
#10980=CARTESIAN_POINT('Ctrl Pts',(7.4485593205266,0.358654244252335,-0.156299477855761));
#10981=CARTESIAN_POINT('Ctrl Pts',(7.72593357368315,0.157347793593328,-0.171999490590986));
#10982=CARTESIAN_POINT('Ctrl Pts',(7.71104009926825,-0.185054253822684,
-0.187699503326212));
#10983=CARTESIAN_POINT('Ctrl Pts',(7.41723396659593,-0.361516217508599,
-0.203399516061437));
#10984=CARTESIAN_POINT('Ctrl Pts',(7.14501874054224,-0.231497029037679,
-0.217218900046785));
#10985=CARTESIAN_POINT('Ctrl Pts',(7.09336669674346,-0.0647065292396766,
-0.225804946453724));
#10986=CARTESIAN_POINT('Ctrl Pts',(7.09297247873625,0.000198368389210352,
-0.229157655282254));
#10987=CARTESIAN_POINT('Ctrl Pts',(7.09284095646985,0.000245638412278346,
-0.120842344717745));
#10988=CARTESIAN_POINT('Ctrl Pts',(7.09260231732278,0.0309143893015408,
-0.122428263772431));
#10989=CARTESIAN_POINT('Ctrl Pts',(7.11080461894951,0.162509776943659,-0.129247520405525));
#10990=CARTESIAN_POINT('Ctrl Pts',(7.2981047634038,0.347285733851148,-0.141300114617028));
#10991=CARTESIAN_POINT('Ctrl Pts',(7.63345360120587,0.276569150443068,-0.157000127352253));
#10992=CARTESIAN_POINT('Ctrl Pts',(7.75946408208296,-0.0421516519758924,
-0.172700140087479));
#10993=CARTESIAN_POINT('Ctrl Pts',(7.56313881583769,-0.323073667897745,
-0.188400152822704));
#10994=CARTESIAN_POINT('Ctrl Pts',(7.22052583282271,-0.314292920077652,
-0.20410016555793));
#10995=CARTESIAN_POINT('Ctrl Pts',(7.09538793769919,-0.11412236888846,-0.214914229522943));
#10996=CARTESIAN_POINT('Ctrl Pts',(7.09218717065892,-0.00679713345771461,
-0.220494955909548));
#10997=CARTESIAN_POINT('Ctrl Pts',(7.0922195431951,-0.000114393265381769,
-0.220842344717745));
#10998=CARTESIAN_POINT('Origin',(7.4,0.,0.220842344717745));
#10999=CARTESIAN_POINT('',(7.09298021495369,-0.000306384811325694,-0.0208423447177452));
#11000=CARTESIAN_POINT('',(7.09227939521384,0.000154311006394861,-0.0291576552822542));
#11001=CARTESIAN_POINT('',(7.09265,5.61065397787037E-15,0.220842344717745));
#11002=CARTESIAN_POINT('',(7.32062007174671,-0.29692229537457,0.));
#11003=CARTESIAN_POINT('Ctrl Pts',(7.32062007174671,-0.29692229537457,0.));
#11004=CARTESIAN_POINT('Ctrl Pts',(7.22298599415769,-0.270820563726849,
-0.00523333757840845));
#11005=CARTESIAN_POINT('Ctrl Pts',(7.11285656998777,-0.167549921885641,
-0.0121807858176569));
#11006=CARTESIAN_POINT('Ctrl Pts',(7.09275376795427,-0.0334730859377096,
-0.0191282340569053));
#11007=CARTESIAN_POINT('Ctrl Pts',(7.09298021495369,-0.000306384811325677,
-0.0208423447177452));
#11008=CARTESIAN_POINT('',(7.47957997103547,-0.297398060845569,-1.37807245336141E-17));
#11009=CARTESIAN_POINT('Origin',(7.4,0.,0.));
#11010=CARTESIAN_POINT('Ctrl Pts',(7.47958090815733,-0.297400289619931,
-6.50521303491303E-19));
#11011=CARTESIAN_POINT('Ctrl Pts',(7.38660350274273,-0.321949666906663,
-0.00499978774624428));
#11012=CARTESIAN_POINT('Ctrl Pts',(7.18097790240557,-0.278640224120542,
-0.0147190061736624));
#11013=CARTESIAN_POINT('Ctrl Pts',(7.09286421205138,-0.0906630570237555,
-0.0244382246010804));
#11014=CARTESIAN_POINT('Ctrl Pts',(7.09227939521384,0.000154311006394901,
-0.0291576552822542));
#11015=CARTESIAN_POINT('Origin',(-7.4,0.,0.220842344717745));
#11016=CARTESIAN_POINT('',(-7.70774490082263,0.000146975295764101,-0.720842344717746));
#11017=CARTESIAN_POINT('',(-7.70687196406169,-1.20609381283741E-5,-0.729157655282255));
#11018=CARTESIAN_POINT('',(-7.70735,5.61059503063532E-15,0.220842344717745));
#11019=CARTESIAN_POINT('',(-7.32062007174671,-0.296922295374569,-0.8));
#11020=CARTESIAN_POINT('Ctrl Pts',(-7.70687196406169,-1.20609381283332E-5,
-0.729157655282254));
#11021=CARTESIAN_POINT('Ctrl Pts',(-7.7068383611135,0.0519523715634962,
-0.731838419874536));
#11022=CARTESIAN_POINT('Ctrl Pts',(-7.66983365783928,0.205395707970149,
-0.739752522045225));
#11023=CARTESIAN_POINT('Ctrl Pts',(-7.42863574303655,0.360721611690756,
-0.752899961794324));
#11024=CARTESIAN_POINT('Ctrl Pts',(-7.1146964728348,0.223016315327006,-0.768599974529548));
#11025=CARTESIAN_POINT('Ctrl Pts',(-7.05707047975879,-0.115238727497404,
-0.784299987264776));
#11026=CARTESIAN_POINT('Ctrl Pts',(-7.22298599415769,-0.270820563726849,
-0.794766662421592));
#11027=CARTESIAN_POINT('Ctrl Pts',(-7.32062007174671,-0.29692229537457,
-0.8));
#11028=CARTESIAN_POINT('',(-7.47958000049154,-0.297398061564379,-0.8));
#11029=CARTESIAN_POINT('Origin',(-7.4,0.,-0.8));
#11030=CARTESIAN_POINT('Ctrl Pts',(-7.70774490082263,0.000146975295764138,
-0.720842344717746));
#11031=CARTESIAN_POINT('Ctrl Pts',(-7.70779645502102,0.00885909073304824,
-0.721295091751952));
#11032=CARTESIAN_POINT('Ctrl Pts',(-7.7035433750236,0.118223822401162,-0.726981176364568));
#11033=CARTESIAN_POINT('Ctrl Pts',(-7.57319886321716,0.317782926109968,
-0.737900598555591));
#11034=CARTESIAN_POINT('Ctrl Pts',(-7.23047488314852,0.319794760031351,
-0.753600611290816));
#11035=CARTESIAN_POINT('Ctrl Pts',(-7.03977528830754,0.0349557588279105,
-0.769300624026042));
#11036=CARTESIAN_POINT('Ctrl Pts',(-7.17010530135127,-0.276350328985862,
-0.784767086929102));
#11037=CARTESIAN_POINT('Ctrl Pts',(-7.38660355712988,-0.321949646446656,
-0.795000212253755));
#11038=CARTESIAN_POINT('Ctrl Pts',(-7.47958093846728,-0.297400292044456,
-0.799999999999999));
#11039=CARTESIAN_POINT('Origin',(-7.4,0.,0.220842344717745));
#11040=CARTESIAN_POINT('',(-7.70689253729186,6.92000104607349E-5,-0.620842344717746));
#11041=CARTESIAN_POINT('',(-7.70767612478914,-0.000188032618375286,-0.629157655282255));
#11042=CARTESIAN_POINT('',(-7.70735,5.61059503063532E-15,0.220842344717745));
#11043=CARTESIAN_POINT('Ctrl Pts',(-7.70767612478914,-0.000188032618375274,
-0.629157655282255));
#11044=CARTESIAN_POINT('Ctrl Pts',(-7.70703140259473,0.0886528337709136,
-0.633771727737419));
#11045=CARTESIAN_POINT('Ctrl Pts',(-7.62022620581121,0.27935843464658,-0.643619137770991));
#11046=CARTESIAN_POINT('Ctrl Pts',(-7.29810477724755,0.347285687712531,
-0.658699885382972));
#11047=CARTESIAN_POINT('Ctrl Pts',(-7.05412291905423,0.106591912271656,
-0.674399898118197));
#11048=CARTESIAN_POINT('Ctrl Pts',(-7.12029939040689,-0.229692046472377,
-0.690099910853423));
#11049=CARTESIAN_POINT('Ctrl Pts',(-7.43727189946158,-0.359992421881043,
-0.705799923588648));
#11050=CARTESIAN_POINT('Ctrl Pts',(-7.67243004463156,-0.200382402588913,
-0.718819171731592));
#11051=CARTESIAN_POINT('Ctrl Pts',(-7.70690396014894,-0.0494916038360727,
-0.726605082296127));
#11052=CARTESIAN_POINT('Ctrl Pts',(-7.70687196406169,-1.20609381283332E-5,
-0.729157655282254));
#11053=CARTESIAN_POINT('Ctrl Pts',(-7.70689253729186,6.92000104607314E-5,
-0.620842344717745));
#11054=CARTESIAN_POINT('Ctrl Pts',(-7.70698770847048,0.0463118050970373,
-0.623228399614835));
#11055=CARTESIAN_POINT('Ctrl Pts',(-7.67563027239018,0.193855832506279,
-0.630847792090332));
#11056=CARTESIAN_POINT('Ctrl Pts',(-7.44855932549587,0.358654280875835,
-0.643700522144239));
#11057=CARTESIAN_POINT('Ctrl Pts',(-7.12764136094462,0.238352663458736,
-0.659400534879464));
#11058=CARTESIAN_POINT('Ctrl Pts',(-7.05095014313138,-0.0956833759672795,
-0.675100547614689));
#11059=CARTESIAN_POINT('Ctrl Pts',(-7.28725499370478,-0.34391658738075,
-0.690800560349915));
#11060=CARTESIAN_POINT('Ctrl Pts',(-7.61493008115263,-0.285496500960074,
-0.706047826050934));
#11061=CARTESIAN_POINT('Ctrl Pts',(-7.70720053610084,-0.0918449175996906,
-0.716061754173544));
#11062=CARTESIAN_POINT('Ctrl Pts',(-7.70774490082263,0.000146975295764138,
-0.720842344717746));
#11063=CARTESIAN_POINT('Origin',(-7.4,0.,0.220842344717745));
#11064=CARTESIAN_POINT('',(-7.70752705531861,-0.000242065129798921,-0.520842344717746));
#11065=CARTESIAN_POINT('',(-7.70730317768915,0.000264518094095117,-0.529157655282254));
#11066=CARTESIAN_POINT('',(-7.70735,5.61059503063532E-15,0.220842344717745));
#11067=CARTESIAN_POINT('Ctrl Pts',(-7.70730317768915,0.000264518094095133,
-0.529157655282254));
#11068=CARTESIAN_POINT('Ctrl Pts',(-7.70752398658218,0.0256450857940224,
-0.530471698021893));
#11069=CARTESIAN_POINT('Ctrl Pts',(-7.69313298964038,0.151860041802368,
-0.53701907833994));
#11070=CARTESIAN_POINT('Ctrl Pts',(-7.51955218823887,0.341611241880446,
-0.548799796236394));
#11071=CARTESIAN_POINT('Ctrl Pts',(-7.18101969602976,0.288164142274201,
-0.56449980897162));
#11072=CARTESIAN_POINT('Ctrl Pts',(-7.03884889133106,-0.0236824478145123,
-0.580199821706845));
#11073=CARTESIAN_POINT('Ctrl Pts',(-7.22052585508497,-0.314292881582478,
-0.595899834442071));
#11074=CARTESIAN_POINT('Ctrl Pts',(-7.56313879548406,-0.323073627560531,
-0.611599847177296));
#11075=CARTESIAN_POINT('Ctrl Pts',(-7.70176606621786,-0.124711731655602,
-0.622685787457357));
#11076=CARTESIAN_POINT('Ctrl Pts',(-7.70776265441629,-0.0121115666782128,
-0.62853839015901));
#11077=CARTESIAN_POINT('Ctrl Pts',(-7.70767612478914,-0.000188032618375274,
-0.629157655282255));
#11078=CARTESIAN_POINT('Ctrl Pts',(-7.70752705531861,-0.000242065129798906,
-0.520842344717745));
#11079=CARTESIAN_POINT('Ctrl Pts',(-7.70680848176124,0.0830296106897686,
-0.525161707477718));
#11080=CARTESIAN_POINT('Ctrl Pts',(-7.62918618390742,0.268374396907059,
-0.534714407816098));
#11081=CARTESIAN_POINT('Ctrl Pts',(-7.31754334759326,0.352408748413955,
-0.549500445732887));
#11082=CARTESIAN_POINT('Ctrl Pts',(-7.06057648784951,0.125629250314373,
-0.565200458468112));
#11083=CARTESIAN_POINT('Ctrl Pts',(-7.10797394984171,-0.213803221083396,
-0.580900471203338));
#11084=CARTESIAN_POINT('Ctrl Pts',(-7.41723396832727,-0.361516254045136,
-0.596600483938562));
#11085=CARTESIAN_POINT('Ctrl Pts',(-7.66638808838325,-0.211872593003345,
-0.609914441776699));
#11086=CARTESIAN_POINT('Ctrl Pts',(-7.70677896938989,-0.0551121660019896,
-0.617995062036427));
#11087=CARTESIAN_POINT('Ctrl Pts',(-7.70689253729186,6.92000104607314E-5,
-0.620842344717745));
#11088=CARTESIAN_POINT('Origin',(-7.4,0.,0.220842344717745));
#11089=CARTESIAN_POINT('',(-7.70746883072654,0.000253844864433833,-0.420842344717745));
#11090=CARTESIAN_POINT('',(-7.70698883508382,-0.000175545619141625,-0.429157655282254));
#11091=CARTESIAN_POINT('',(-7.70735,5.61059503063532E-15,0.220842344717745));
#11092=CARTESIAN_POINT('Ctrl Pts',(-7.70698883508383,-0.000175545619141616,
-0.429157655282254));
#11093=CARTESIAN_POINT('Ctrl Pts',(-7.70665371353763,0.0627096523718999,
-0.432405005884775));
#11094=CARTESIAN_POINT('Ctrl Pts',(-7.65747280757301,0.227420133227449,
-0.440885694065705));
#11095=CARTESIAN_POINT('Ctrl Pts',(-7.38994851155463,0.361787133550707,
-0.454599719825042));
#11096=CARTESIAN_POINT('Ctrl Pts',(-7.09269613963708,0.191194402405521,
-0.470299732560268));
#11097=CARTESIAN_POINT('Ctrl Pts',(-7.07100608667554,-0.15084418271379,
-0.485999745295493));
#11098=CARTESIAN_POINT('Ctrl Pts',(-7.34432803357192,-0.357619343872072,
-0.501699758030719));
#11099=CARTESIAN_POINT('Ctrl Pts',(-7.64051707522517,-0.253247347882201,
-0.516085728026305));
#11100=CARTESIAN_POINT('Ctrl Pts',(-7.70664458788177,-0.0754361611842396,
-0.525238360443484));
#11101=CARTESIAN_POINT('Ctrl Pts',(-7.70730317768915,0.000264518094095133,
-0.529157655282254));
#11102=CARTESIAN_POINT('Ctrl Pts',(-7.70746883072654,0.000253844864433892,
-0.420842344717745));
#11103=CARTESIAN_POINT('Ctrl Pts',(-7.70764252858464,0.0199148934326357,
-0.421861677762192));
#11104=CARTESIAN_POINT('Ctrl Pts',(-7.69704050311101,0.140330871783531,
-0.428114348385046));
#11105=CARTESIAN_POINT('Ctrl Pts',(-7.53833505704833,0.334446467171126,
-0.43960035658631));
#11106=CARTESIAN_POINT('Ctrl Pts',(-7.19735713758398,0.299878138056265,
-0.455300369321535));
#11107=CARTESIAN_POINT('Ctrl Pts',(-7.03809101690294,-0.0035937942090703,
-0.47100038205676));
#11108=CARTESIAN_POINT('Ctrl Pts',(-7.20335215339251,-0.30384313701778,
-0.486700394791986));
#11109=CARTESIAN_POINT('Ctrl Pts',(-7.54494930042661,-0.331633423345088,
-0.50240040752721));
#11110=CARTESIAN_POINT('Ctrl Pts',(-7.6983485357738,-0.136213625138345,
-0.513781057502464));
#11111=CARTESIAN_POINT('Ctrl Pts',(-7.7076791050938,-0.0178623065907353,
-0.519928369899309));
#11112=CARTESIAN_POINT('Ctrl Pts',(-7.70752705531861,-0.000242065129798906,
-0.520842344717745));
#11113=CARTESIAN_POINT('Origin',(-7.4,0.,0.220842344717745));
#11114=CARTESIAN_POINT('',(-7.70690963115052,-9.95083586281809E-5,-0.320842344717745));
#11115=CARTESIAN_POINT('',(-7.7078347863644,-1.80303430137119E-5,-0.329157655282254));
#11116=CARTESIAN_POINT('',(-7.70735,5.61059503063532E-15,0.220842344717745));
#11117=CARTESIAN_POINT('Ctrl Pts',(-7.70783478636441,-1.80303430137095E-5,
-0.329157655282254));
#11118=CARTESIAN_POINT('Ctrl Pts',(-7.70774834240926,0.0995954626777301,
-0.334338313747658));
#11119=CARTESIAN_POINT('Ctrl Pts',(-7.60149871047448,0.299994052557417,
-0.34475230979147));
#11120=CARTESIAN_POINT('Ctrl Pts',(-7.26166497730884,0.334446384107517,
-0.36039964341369));
#11121=CARTESIAN_POINT('Ctrl Pts',(-7.04473348450178,0.0691134233972956,
-0.376099656148916));
#11122=CARTESIAN_POINT('Ctrl Pts',(-7.14637288440692,-0.258194207068779,
-0.391799668884141));
#11123=CARTESIAN_POINT('Ctrl Pts',(-7.47544215207399,-0.353976615097665,
-0.407499681619366));
#11124=CARTESIAN_POINT('Ctrl Pts',(-7.68279036168308,-0.178186556672294,
-0.419952343752071));
#11125=CARTESIAN_POINT('Ctrl Pts',(-7.70719378585987,-0.0386343384853514,
-0.427171668306367));
#11126=CARTESIAN_POINT('Ctrl Pts',(-7.70698883508383,-0.000175545619141616,
-0.429157655282254));
#11127=CARTESIAN_POINT('Ctrl Pts',(-7.70690963115052,-9.95083586281427E-5,
-0.320842344717745));
#11128=CARTESIAN_POINT('Ctrl Pts',(-7.70673966230461,0.0571157403095281,
-0.323794985625074));
#11129=CARTESIAN_POINT('Ctrl Pts',(-7.66412291034569,0.215975982062961,
-0.331980964110812));
#11130=CARTESIAN_POINT('Ctrl Pts',(-7.41005149094087,0.36178722340353,-0.345400280174957));
#11131=CARTESIAN_POINT('Ctrl Pts',(-7.10378577645897,0.207961922416443,
-0.361100292910183));
#11132=CARTESIAN_POINT('Ctrl Pts',(-7.06313819816462,-0.132344829277446,
-0.376800305645408));
#11133=CARTESIAN_POINT('Ctrl Pts',(-7.32455782918916,-0.35397670301188,
-0.392500318380633));
#11134=CARTESIAN_POINT('Ctrl Pts',(-7.6322621473956,-0.264413004865462,
-0.407180998071413));
#11135=CARTESIAN_POINT('Ctrl Pts',(-7.70675074985441,-0.081026506302691,
-0.416628340183783));
#11136=CARTESIAN_POINT('Ctrl Pts',(-7.70746883072654,0.000253844864433892,
-0.420842344717745));
#11137=CARTESIAN_POINT('Origin',(-7.4,0.,0.220842344717745));
#11138=CARTESIAN_POINT('',(-7.70778049527,-0.000114393321009997,-0.220842344717745));
#11139=CARTESIAN_POINT('',(-7.70702747598399,0.000198368355311817,-0.229157655282254));
#11140=CARTESIAN_POINT('',(-7.70735,5.61059503063532E-15,0.220842344717745));
#11141=CARTESIAN_POINT('Ctrl Pts',(-7.70702747598399,0.000198368355311809,
-0.229157655282254));
#11142=CARTESIAN_POINT('Ctrl Pts',(-7.70724860392715,0.0366053469345374,
-0.231038284032132));
#11143=CARTESIAN_POINT('Ctrl Pts',(-7.68454864144738,0.17405755161616,-0.238152250360418));
#11144=CARTESIAN_POINT('Ctrl Pts',(-7.48245663192943,0.352408660865427,
-0.250499554267113));
#11145=CARTESIAN_POINT('Ctrl Pts',(-7.15155018414657,0.263179885173358,
-0.266199567002338));
#11146=CARTESIAN_POINT('Ctrl Pts',(-7.04343106924415,-0.0620448231745263,
-0.281899579737564));
#11147=CARTESIAN_POINT('Ctrl Pts',(-7.25505073557315,-0.331633340976559,
-0.297599592472789));
#11148=CARTESIAN_POINT('Ctrl Pts',(-7.59664779776768,-0.303843061556337,
-0.313299605208015));
#11149=CARTESIAN_POINT('Ctrl Pts',(-7.7073763710065,-0.102669439907453,
-0.323818959477836));
#11150=CARTESIAN_POINT('Ctrl Pts',(-7.70783566536288,-0.00103094221332684,
-0.329104976169249));
#11151=CARTESIAN_POINT('Ctrl Pts',(-7.70783478636441,-1.80303430137095E-5,
-0.329157655282254));
#11152=CARTESIAN_POINT('Ctrl Pts',(-7.70778049527,-0.000114393321009984,
-0.220842344717745));
#11153=CARTESIAN_POINT('Ctrl Pts',(-7.70732518245543,0.0938769199589478,
-0.225728293487957));
#11154=CARTESIAN_POINT('Ctrl Pts',(-7.61148976398448,0.289346819956445,
-0.235847579836577));
#11155=CARTESIAN_POINT('Ctrl Pts',(-7.28044778202723,0.341611326648396,
-0.251200203763605));
#11156=CARTESIAN_POINT('Ctrl Pts',(-7.04911880083639,0.0887322557395692,
-0.266900216498831));
#11157=CARTESIAN_POINT('Ctrl Pts',(-7.13242836981262,-0.243713865431744,
-0.282600229234056));
#11158=CARTESIAN_POINT('Ctrl Pts',(-7.45567198026117,-0.357619432680664,
-0.298300241969282));
#11159=CARTESIAN_POINT('Ctrl Pts',(-7.67759137674685,-0.189731637750237,
-0.311047613797178));
#11160=CARTESIAN_POINT('Ctrl Pts',(-7.70704091951006,-0.0442940552974542,
-0.318561648046666));
#11161=CARTESIAN_POINT('Ctrl Pts',(-7.70690963115052,-9.95083586281427E-5,
-0.320842344717745));
#11162=CARTESIAN_POINT('Origin',(-7.4,0.,0.220842344717745));
#11163=CARTESIAN_POINT('',(-7.70715908192673,0.00024563889874174,-0.120842344717745));
#11164=CARTESIAN_POINT('',(-7.70724559592217,-0.000260666439420178,-0.129157655282254));
#11165=CARTESIAN_POINT('',(-7.70735,5.61059503063532E-15,0.220842344717745));
#11166=CARTESIAN_POINT('Ctrl Pts',(-7.70724559592217,-0.000260666439420156,
-0.129157655282254));
#11167=CARTESIAN_POINT('Ctrl Pts',(-7.70662480337493,0.0734403154642453,
-0.132971591895015));
#11168=CARTESIAN_POINT('Ctrl Pts',(-7.64334514522135,0.249228787607049,
-0.142018866086183));
#11169=CARTESIAN_POINT('Ctrl Pts',(-7.351440686739,0.358654190708449,-0.156299477855761));
#11170=CARTESIAN_POINT('Ctrl Pts',(-7.07406647433649,0.15734777073398,-0.171999490590986));
#11171=CARTESIAN_POINT('Ctrl Pts',(-7.08895994662689,-0.185054226714597,
-0.187699503326211));
#11172=CARTESIAN_POINT('Ctrl Pts',(-7.38276603593497,-0.36151616409523,
-0.203399516061437));
#11173=CARTESIAN_POINT('Ctrl Pts',(-7.65498122185629,-0.231496994929852,
-0.217218900046784));
#11174=CARTESIAN_POINT('Ctrl Pts',(-7.70663325803569,-0.0647065197097194,
-0.225804946453724));
#11175=CARTESIAN_POINT('Ctrl Pts',(-7.70702747598399,0.000198368355311809,
-0.229157655282254));
#11176=CARTESIAN_POINT('Ctrl Pts',(-7.70715908192673,0.000245638898741782,
-0.120842344717745));
#11177=CARTESIAN_POINT('Ctrl Pts',(-7.7073977208252,0.0309143927359499,
-0.122428263772431));
#11178=CARTESIAN_POINT('Ctrl Pts',(-7.68919541585723,0.162509793267262,
-0.129247520405525));
#11179=CARTESIAN_POINT('Ctrl Pts',(-7.50189525062872,0.347285780617978,
-0.141300114617028));
#11180=CARTESIAN_POINT('Ctrl Pts',(-7.16654636885183,0.276569183243976,
-0.157000127352254));
#11181=CARTESIAN_POINT('Ctrl Pts',(-7.04053587339322,-0.0421516562996225,
-0.172700140087479));
#11182=CARTESIAN_POINT('Ctrl Pts',(-7.23686116352416,-0.323073708797981,
-0.188400152822704));
#11183=CARTESIAN_POINT('Ctrl Pts',(-7.5794741897514,-0.314292959115147,
-0.204100165557929));
#11184=CARTESIAN_POINT('Ctrl Pts',(-7.70461210038305,-0.114122383172389,
-0.214914229522943));
#11185=CARTESIAN_POINT('Ctrl Pts',(-7.70781286781081,-0.00679713434773683,
-0.220494955909549));
#11186=CARTESIAN_POINT('Ctrl Pts',(-7.70778049527,-0.000114393321009984,
-0.220842344717745));
#11187=CARTESIAN_POINT('Origin',(-7.4,0.,0.220842344717745));
#11188=CARTESIAN_POINT('',(-7.70701976654778,-0.00030617080607008,-0.0208423447177452));
#11189=CARTESIAN_POINT('',(-7.70772056490863,0.000154295167761162,-0.0291576552822542));
#11190=CARTESIAN_POINT('',(-7.70735,5.61059503063532E-15,0.220842344717745));
#11191=CARTESIAN_POINT('',(-7.47937992825329,-0.29692229537457,0.));
#11192=CARTESIAN_POINT('Ctrl Pts',(-7.47937992825329,-0.29692229537457,
0.));
#11193=CARTESIAN_POINT('Ctrl Pts',(-7.57701400584231,-0.270820563726849,
-0.00523333757840845));
#11194=CARTESIAN_POINT('Ctrl Pts',(-7.68714337778258,-0.167549582709018,
-0.0121807858176569));
#11195=CARTESIAN_POINT('Ctrl Pts',(-7.7072462053552,-0.0334728379797751,
-0.0191282340569053));
#11196=CARTESIAN_POINT('Ctrl Pts',(-7.70701976654778,-0.000306170806070059,
-0.0208423447177452));
#11197=CARTESIAN_POINT('',(-7.3204200723426,-0.297398060139812,-2.068740934409E-17));
#11198=CARTESIAN_POINT('Origin',(-7.4,0.,0.));
#11199=CARTESIAN_POINT('Ctrl Pts',(-7.32041913648099,-0.297400286396329,
-1.35525271560688E-19));
#11200=CARTESIAN_POINT('Ctrl Pts',(-7.413396577125,-0.321949697150244,-0.00499978774624428));
#11201=CARTESIAN_POINT('Ctrl Pts',(-7.61902199122377,-0.278640078019593,
-0.0147190061736623));
#11202=CARTESIAN_POINT('Ctrl Pts',(-7.70713573379311,-0.0906630403545633,
-0.0244382246010804));
#11203=CARTESIAN_POINT('Ctrl Pts',(-7.70772056490863,0.000154295167761189,
-0.0291576552822542));
#11204=CARTESIAN_POINT('Origin',(0.,-7.4,0.220842344717745));
#11205=CARTESIAN_POINT('',(-0.307744883519712,-7.39985302304706,-0.720842344717745));
#11206=CARTESIAN_POINT('',(-0.306872009074495,-7.40001207497238,-0.729157655282255));
#11207=CARTESIAN_POINT('',(-0.30735,-7.4,0.220842344717745));
#11208=CARTESIAN_POINT('',(0.079379928253284,-7.69692229537457,-0.8));
#11209=CARTESIAN_POINT('Ctrl Pts',(-0.306872009074495,-7.40001207497238,
-0.729157655282255));
#11210=CARTESIAN_POINT('Ctrl Pts',(-0.306838407663091,-7.34804764485915,
-0.731838419874537));
#11211=CARTESIAN_POINT('Ctrl Pts',(-0.269833704177636,-7.1946043063299,
-0.739752522045226));
#11212=CARTESIAN_POINT('Ctrl Pts',(-0.0286357500746574,-7.03927819062664,
-0.752899961794323));
#11213=CARTESIAN_POINT('Ctrl Pts',(0.285303607599647,-7.17698390717715,
-0.76859997452955));
#11214=CARTESIAN_POINT('Ctrl Pts',(0.342929427239765,-7.51523812385981,
-0.784299987264775));
#11215=CARTESIAN_POINT('Ctrl Pts',(0.177014005842305,-7.67082056372685,
-0.794766662421592));
#11216=CARTESIAN_POINT('Ctrl Pts',(0.0793799282532836,-7.69692229537457,
-0.8));
#11217=CARTESIAN_POINT('',(-0.0795799836281317,-7.69739806112894,-0.8));
#11218=CARTESIAN_POINT('Origin',(0.,-7.4,-0.8));
#11219=CARTESIAN_POINT('Ctrl Pts',(-0.307744883519712,-7.39985302304706,
-0.720842344717745));
#11220=CARTESIAN_POINT('Ctrl Pts',(-0.30779643769355,-7.39114090815323,
-0.721295091751952));
#11221=CARTESIAN_POINT('Ctrl Pts',(-0.303543357565344,-7.28177618361729,
-0.726981176364567));
#11222=CARTESIAN_POINT('Ctrl Pts',(-0.173198849645488,-7.08221710163593,
-0.737900598555592));
#11223=CARTESIAN_POINT('Ctrl Pts',(0.169525099592154,-7.08020524213913,
-0.753600611290816));
#11224=CARTESIAN_POINT('Ctrl Pts',(0.360224706479889,-7.36504427094214,
-0.769300624026043));
#11225=CARTESIAN_POINT('Ctrl Pts',(0.229894653244661,-7.67635026824636,
-0.784767086929102));
#11226=CARTESIAN_POINT('Ctrl Pts',(0.0133964740216469,-7.72194965815218,
-0.795000212253756));
#11227=CARTESIAN_POINT('Ctrl Pts',(-0.0795809211152242,-7.69740029063291,
-0.8));
#11228=CARTESIAN_POINT('Origin',(0.,-7.4,0.220842344717745));
#11229=CARTESIAN_POINT('',(-0.306892519549444,-7.39993079996377,-0.620842344717746));
#11230=CARTESIAN_POINT('',(-0.307676170073155,-7.40018803246927,-0.629157655282255));
#11231=CARTESIAN_POINT('',(-0.30735,-7.4,0.220842344717745));
#11232=CARTESIAN_POINT('Ctrl Pts',(-0.307676170073155,-7.40018803246927,
-0.629157655282255));
#11233=CARTESIAN_POINT('Ctrl Pts',(-0.307031447936131,-7.31134715334416,
-0.633771727737419));
#11234=CARTESIAN_POINT('Ctrl Pts',(-0.22022623908268,-7.12064152602881,
-0.643619137770991));
#11235=CARTESIAN_POINT('Ctrl Pts',(0.101895239308332,-7.05271425710996,
-0.658699885382973));
#11236=CARTESIAN_POINT('Ctrl Pts',(0.345877129402089,-7.29340807937902,
-0.674399898118197));
#11237=CARTESIAN_POINT('Ctrl Pts',(0.279700654926715,-7.62969206672302,
-0.690099910853423));
#11238=CARTESIAN_POINT('Ctrl Pts',(-0.0372719110426151,-7.75999249994725,
-0.705799923588648));
#11239=CARTESIAN_POINT('Ctrl Pts',(-0.272430079269896,-7.60038239881887,
-0.718819171731592));
#11240=CARTESIAN_POINT('Ctrl Pts',(-0.306904003698451,-7.44949161559615,
-0.726605082296128));
#11241=CARTESIAN_POINT('Ctrl Pts',(-0.306872009074495,-7.40001207497238,
-0.729157655282255));
#11242=CARTESIAN_POINT('Ctrl Pts',(-0.306892519549444,-7.39993079996377,
-0.620842344717746));
#11243=CARTESIAN_POINT('Ctrl Pts',(-0.306987690724187,-7.35368819753831,
-0.623228399614835));
#11244=CARTESIAN_POINT('Ctrl Pts',(-0.27563025645925,-7.20614417863957,
-0.630847792090333));
#11245=CARTESIAN_POINT('Ctrl Pts',(-0.0485593226474429,-7.04134574011728,
-0.643700522144239));
#11246=CARTESIAN_POINT('Ctrl Pts',(0.272358623219876,-7.16164734985291,
-0.659400534879465));
#11247=CARTESIAN_POINT('Ctrl Pts',(0.349049836864763,-7.49568337130869,
-0.675100547614689));
#11248=CARTESIAN_POINT('Ctrl Pts',(0.11274499939327,-7.74391656588417,-0.690800560349915));
#11249=CARTESIAN_POINT('Ctrl Pts',(-0.21493006795272,-7.68549648725022,
-0.706047826050934));
#11250=CARTESIAN_POINT('Ctrl Pts',(-0.307200519057126,-7.4918449102041,
-0.716061754173544));
#11251=CARTESIAN_POINT('Ctrl Pts',(-0.307744883519712,-7.39985302304706,
-0.720842344717745));
#11252=CARTESIAN_POINT('Origin',(0.,-7.4,0.220842344717745));
#11253=CARTESIAN_POINT('',(-0.307527037534926,-7.40024206511592,-0.520842344717746));
#11254=CARTESIAN_POINT('',(-0.30730322300603,-7.39973548185956,-0.529157655282254));
#11255=CARTESIAN_POINT('',(-0.30735,-7.4,0.220842344717745));
#11256=CARTESIAN_POINT('Ctrl Pts',(-0.30730322300603,-7.39973548185956,
-0.529157655282254));
#11257=CARTESIAN_POINT('Ctrl Pts',(-0.307524031931375,-7.37435491041612,
-0.530471698021893));
#11258=CARTESIAN_POINT('Ctrl Pts',(-0.293133032867834,-7.248139935795,-0.537019078339939));
#11259=CARTESIAN_POINT('Ctrl Pts',(-0.119552205895206,-7.05838870778368,
-0.548799796236395));
#11260=CARTESIAN_POINT('Ctrl Pts',(0.21898033631151,-7.11183581514136,-0.56449980897162));
#11261=CARTESIAN_POINT('Ctrl Pts',(0.361151161846345,-7.42368245147158,
-0.580199821706845));
#11262=CARTESIAN_POINT('Ctrl Pts',(0.179474171539626,-7.71429292762124,
-0.595899834442071));
#11263=CARTESIAN_POINT('Ctrl Pts',(-0.16313881982596,-7.72307367580168,
-0.611599847177296));
#11264=CARTESIAN_POINT('Ctrl Pts',(-0.301766110448845,-7.52471174942935,
-0.622685787457358));
#11265=CARTESIAN_POINT('Ctrl Pts',(-0.307762699692601,-7.41211156823841,
-0.62853839015901));
#11266=CARTESIAN_POINT('Ctrl Pts',(-0.307676170073155,-7.40018803246927,
-0.629157655282255));
#11267=CARTESIAN_POINT('Ctrl Pts',(-0.307527037534926,-7.40024206511592,
-0.520842344717745));
#11268=CARTESIAN_POINT('Ctrl Pts',(-0.306808464019153,-7.31697039411127,
-0.525161707477718));
#11269=CARTESIAN_POINT('Ctrl Pts',(-0.229186170654196,-7.13162561861014,
-0.534714407816098));
#11270=CARTESIAN_POINT('Ctrl Pts',(0.0824566476388583,-7.04759127197059,
-0.549500445732887));
#11271=CARTESIAN_POINT('Ctrl Pts',(0.3394234925214,-7.27437075694011,-0.565200458468112));
#11272=CARTESIAN_POINT('Ctrl Pts',(0.292026033272937,-7.61380320873943,
-0.580900471203338));
#11273=CARTESIAN_POINT('Ctrl Pts',(-0.0172339673348224,-7.76151623310164,
-0.596600483938563));
#11274=CARTESIAN_POINT('Ctrl Pts',(-0.266388072971644,-7.61187258080603,
-0.609914441776699));
#11275=CARTESIAN_POINT('Ctrl Pts',(-0.306778951652101,-7.4551121628007,
-0.617995062036427));
#11276=CARTESIAN_POINT('Ctrl Pts',(-0.306892519549444,-7.39993079996377,
-0.620842344717746));
#11277=CARTESIAN_POINT('Origin',(0.,-7.4,0.220842344717745));
#11278=CARTESIAN_POINT('',(-0.307468812946229,-7.39974615515026,-0.420842344717745));
#11279=CARTESIAN_POINT('',(-0.306988880358463,-7.40017554564499,-0.429157655282254));
#11280=CARTESIAN_POINT('',(-0.30735,-7.4,0.220842344717745));
#11281=CARTESIAN_POINT('Ctrl Pts',(-0.306988880358463,-7.40017554564498,
-0.429157655282254));
#11282=CARTESIAN_POINT('Ctrl Pts',(-0.306653758762801,-7.33729033837957,
-0.432405005884775));
#11283=CARTESIAN_POINT('Ctrl Pts',(-0.25747284554488,-7.17257983323238,
-0.440885694065705));
#11284=CARTESIAN_POINT('Ctrl Pts',(0.010051489927223,-7.03821281309385,
-0.454599719825043));
#11285=CARTESIAN_POINT('Ctrl Pts',(0.307303905685085,-7.20880556939548,
-0.470299732560268));
#11286=CARTESIAN_POINT('Ctrl Pts',(0.328993961842462,-7.55084420496352,
-0.485999745295494));
#11287=CARTESIAN_POINT('Ctrl Pts',(0.0556719746423119,-7.75761939660742,
-0.501699758030718));
#11288=CARTESIAN_POINT('Ctrl Pts',(-0.240517110702747,-7.65324738524168,
-0.516085728026306));
#11289=CARTESIAN_POINT('Ctrl Pts',(-0.306644633102251,-7.47543617230339,
-0.525238360443484));
#11290=CARTESIAN_POINT('Ctrl Pts',(-0.30730322300603,-7.39973548185956,
-0.529157655282254));
#11291=CARTESIAN_POINT('Ctrl Pts',(-0.307468812946229,-7.39974615515026,
-0.420842344717745));
#11292=CARTESIAN_POINT('Ctrl Pts',(-0.307642510794279,-7.38008510771902,
-0.421861677762192));
#11293=CARTESIAN_POINT('Ctrl Pts',(-0.29704048593374,-7.25966913633154,
-0.428114348385046));
#11294=CARTESIAN_POINT('Ctrl Pts',(-0.138335049048699,-7.06555355216919,
-0.43960035658631));
#11295=CARTESIAN_POINT('Ctrl Pts',(0.202642850697595,-7.1001218792852,-0.455300369321535));
#11296=CARTESIAN_POINT('Ctrl Pts',(0.361908962168568,-7.40359379400104,
-0.47100038205676));
#11297=CARTESIAN_POINT('Ctrl Pts',(0.196647835235759,-7.70384311944753,
-0.486700394791986));
#11298=CARTESIAN_POINT('Ctrl Pts',(-0.144949292044521,-7.73163340416662,
-0.502400407527211));
#11299=CARTESIAN_POINT('Ctrl Pts',(-0.298348518520842,-7.53621361726224,
-0.513781057502464));
#11300=CARTESIAN_POINT('Ctrl Pts',(-0.307679087301317,-7.41786230555802,
-0.519928369899309));
#11301=CARTESIAN_POINT('Ctrl Pts',(-0.307527037534926,-7.40024206511592,
-0.520842344717745));
#11302=CARTESIAN_POINT('Origin',(0.,-7.4,0.220842344717745));
#11303=CARTESIAN_POINT('',(-0.306909613402721,-7.40009950835258,-0.320842344717745));
#11304=CARTESIAN_POINT('',(-0.307834831763841,-7.40001803034581,-0.329157655282254));
#11305=CARTESIAN_POINT('',(-0.30735,-7.4,0.220842344717745));
#11306=CARTESIAN_POINT('Ctrl Pts',(-0.307834831763841,-7.40001803034581,
-0.329157655282254));
#11307=CARTESIAN_POINT('Ctrl Pts',(-0.307748387795955,-7.3004045226342,
-0.334338313747658));
#11308=CARTESIAN_POINT('Ctrl Pts',(-0.201498740191458,-7.10000590319923,
-0.34475230979147));
#11309=CARTESIAN_POINT('Ctrl Pts',(0.13833504309277,-7.06555356656853,-0.36039964341369));
#11310=CARTESIAN_POINT('Ctrl Pts',(0.355266567892898,-7.33088656640977,
-0.376099656148916));
#11311=CARTESIAN_POINT('Ctrl Pts',(0.253627152997932,-7.65819424514732,
-0.391799668884141));
#11312=CARTESIAN_POINT('Ctrl Pts',(-0.0754421632001089,-7.75397666730194,
-0.407499681619367));
#11313=CARTESIAN_POINT('Ctrl Pts',(-0.282790403389065,-7.57818658295138,
-0.419952343752071));
#11314=CARTESIAN_POINT('Ctrl Pts',(-0.307193831164762,-7.43863434418313,
-0.427171668306367));
#11315=CARTESIAN_POINT('Ctrl Pts',(-0.306988880358463,-7.40017554564498,
-0.429157655282254));
#11316=CARTESIAN_POINT('Ctrl Pts',(-0.306909613402721,-7.40009950835258,
-0.320842344717745));
#11317=CARTESIAN_POINT('Ctrl Pts',(-0.30673964456656,-7.3428842629932,-0.323794985625074));
#11318=CARTESIAN_POINT('Ctrl Pts',(-0.264122895071672,-7.18402403042701,
-0.331980964110812));
#11319=CARTESIAN_POINT('Ctrl Pts',(-0.0100514903598289,-7.03821279751757,
-0.345400280174958));
#11320=CARTESIAN_POINT('Ctrl Pts',(0.296214206411665,-7.19203808960976,
-0.361100292910183));
#11321=CARTESIAN_POINT('Ctrl Pts',(0.336861782355269,-7.53234482162411,
-0.376800305645408));
#11322=CARTESIAN_POINT('Ctrl Pts',(0.0754421664482044,-7.75397668254217,
-0.392500318380634));
#11323=CARTESIAN_POINT('Ctrl Pts',(-0.232262133964356,-7.66441298957495,
-0.407180998071413));
#11324=CARTESIAN_POINT('Ctrl Pts',(-0.306750732115625,-7.4810265016171,
-0.416628340183783));
#11325=CARTESIAN_POINT('Ctrl Pts',(-0.307468812946229,-7.39974615515026,
-0.420842344717745));
#11326=CARTESIAN_POINT('Origin',(0.,-7.4,0.220842344717745));
#11327=CARTESIAN_POINT('',(-0.30778047748176,-7.40011439329532,-0.220842344717745));
#11328=CARTESIAN_POINT('',(-0.307027521263749,-7.39980163161079,-0.229157655282254));
#11329=CARTESIAN_POINT('',(-0.30735,-7.4,0.220842344717745));
#11330=CARTESIAN_POINT('Ctrl Pts',(-0.307027521263749,-7.39980163161079,
-0.229157655282254));
#11331=CARTESIAN_POINT('Ctrl Pts',(-0.30724864923996,-7.36339464766693,
-0.231038284032132));
#11332=CARTESIAN_POINT('Ctrl Pts',(-0.284548683414164,-7.22594242273193,
-0.238152250360418));
#11333=CARTESIAN_POINT('Ctrl Pts',(-0.0824566440890477,-7.04759128714739,
-0.250499554267113));
#11334=CARTESIAN_POINT('Ctrl Pts',(0.248449852494269,-7.13682007602022,
-0.266199567002339));
#11335=CARTESIAN_POINT('Ctrl Pts',(0.356568983342811,-7.46204483232109,
-0.281899579737564));
#11336=CARTESIAN_POINT('Ctrl Pts',(0.144949285803845,-7.73163338988777,
-0.297599592472789));
#11337=CARTESIAN_POINT('Ctrl Pts',(-0.196647826769216,-7.70384310636604,
-0.313299605208015));
#11338=CARTESIAN_POINT('Ctrl Pts',(-0.30737641633832,-7.50266945504914,
-0.323818959477836));
#11339=CARTESIAN_POINT('Ctrl Pts',(-0.307835710762444,-7.40103094236551,
-0.329104976169249));
#11340=CARTESIAN_POINT('Ctrl Pts',(-0.307834831763841,-7.40001803034581,
-0.329157655282254));
#11341=CARTESIAN_POINT('Ctrl Pts',(-0.30778047748176,-7.40011439329532,
-0.220842344717745));
#11342=CARTESIAN_POINT('Ctrl Pts',(-0.307325164697339,-7.3061230854425,
-0.225728293487957));
#11343=CARTESIAN_POINT('Ctrl Pts',(-0.211489751737109,-7.11065319680823,
-0.235847579836577));
#11344=CARTESIAN_POINT('Ctrl Pts',(0.119552211049655,-7.05838869308885,
-0.251200203763606));
#11345=CARTESIAN_POINT('Ctrl Pts',(0.350881178877997,-7.31126774940073,
-0.266900216498831));
#11346=CARTESIAN_POINT('Ctrl Pts',(0.267571614711511,-7.64371385133353,
-0.282600229234056));
#11347=CARTESIAN_POINT('Ctrl Pts',(-0.0556719770403169,-7.75761941200269,
-0.298300241969282));
#11348=CARTESIAN_POINT('Ctrl Pts',(-0.277591360694641,-7.58973162677787,
-0.311047613797178));
#11349=CARTESIAN_POINT('Ctrl Pts',(-0.307040901754737,-7.44429405273561,
-0.318561648046666));
#11350=CARTESIAN_POINT('Ctrl Pts',(-0.306909613402721,-7.40009950835258,
-0.320842344717745));
#11351=CARTESIAN_POINT('Origin',(0.,-7.4,0.220842344717745));
#11352=CARTESIAN_POINT('',(-0.307159064170147,-7.39975436132604,-0.120842344717745));
#11353=CARTESIAN_POINT('',(-0.307245641089215,-7.40026066578654,-0.129157655282254));
#11354=CARTESIAN_POINT('',(-0.30735,-7.4,0.220842344717745));
#11355=CARTESIAN_POINT('Ctrl Pts',(-0.307245641089215,-7.40026066578654,
-0.129157655282254));
#11356=CARTESIAN_POINT('Ctrl Pts',(-0.306624848470386,-7.32655967317157,
-0.132971591895015));
#11357=CARTESIAN_POINT('Ctrl Pts',(-0.24334518130105,-7.15077117668026,
-0.142018866086184));
#11358=CARTESIAN_POINT('Ctrl Pts',(0.0485593205265976,-7.04134575574766,
-0.156299477855761));
#11359=CARTESIAN_POINT('Ctrl Pts',(0.32593357368315,-7.24265220640667,-0.171999490590986));
#11360=CARTESIAN_POINT('Ctrl Pts',(0.311040099268243,-7.58505425382268,
-0.187699503326212));
#11361=CARTESIAN_POINT('Ctrl Pts',(0.017233966595936,-7.7615162175086,-0.203399516061437));
#11362=CARTESIAN_POINT('Ctrl Pts',(-0.25498125945776,-7.63149702903767,
-0.217218900046785));
#11363=CARTESIAN_POINT('Ctrl Pts',(-0.306633303256541,-7.46470652923967,
-0.225804946453724));
#11364=CARTESIAN_POINT('Ctrl Pts',(-0.307027521263749,-7.39980163161079,
-0.229157655282254));
#11365=CARTESIAN_POINT('Ctrl Pts',(-0.307159064170147,-7.39975436132604,
-0.120842344717745));
#11366=CARTESIAN_POINT('Ctrl Pts',(-0.307397703183449,-7.3690856088527,
-0.122428263772431));
#11367=CARTESIAN_POINT('Ctrl Pts',(-0.289195399760154,-7.23749021428436,
-0.129247520405525));
#11368=CARTESIAN_POINT('Ctrl Pts',(-0.101895244140074,-7.05271424100694,
-0.141300114617028));
#11369=CARTESIAN_POINT('Ctrl Pts',(0.233453617301762,-7.1234308319262,-0.157000127352253));
#11370=CARTESIAN_POINT('Ctrl Pts',(0.359464106016436,-7.44215165429935,
-0.172700140087479));
#11371=CARTESIAN_POINT('Ctrl Pts',(0.163138826931865,-7.72307368988404,
-0.188400152822704));
#11372=CARTESIAN_POINT('Ctrl Pts',(-0.179474179312067,-7.714292941062,-0.204100165557929));
#11373=CARTESIAN_POINT('Ctrl Pts',(-0.304612082771875,-7.51412237656679,
-0.214914229522943));
#11374=CARTESIAN_POINT('Ctrl Pts',(-0.307812850020437,-7.40679713393618,
-0.220494955909548));
#11375=CARTESIAN_POINT('Ctrl Pts',(-0.30778047748176,-7.40011439329532,
-0.220842344717745));
#11376=CARTESIAN_POINT('Origin',(0.,-7.4,0.220842344717745));
#11377=CARTESIAN_POINT('',(-0.307019775097118,-7.40030626975107,-0.0208423447177452));
#11378=CARTESIAN_POINT('',(-0.307720604786163,-7.39984568899361,-0.0291576552822545));
#11379=CARTESIAN_POINT('',(-0.30735,-7.4,0.220842344717745));
#11380=CARTESIAN_POINT('',(-0.0793799282532844,-7.69692229537457,0.));
#11381=CARTESIAN_POINT('Ctrl Pts',(-0.0793799282532839,-7.69692229537457,
2.77555756156289E-17));
#11382=CARTESIAN_POINT('Ctrl Pts',(-0.177014005842305,-7.67082056372685,
-0.00523333757840842));
#11383=CARTESIAN_POINT('Ctrl Pts',(-0.287143401920737,-7.56754973948506,
-0.0121807858176568));
#11384=CARTESIAN_POINT('Ctrl Pts',(-0.307246217690486,-7.43347295261345,
-0.0191282340569052));
#11385=CARTESIAN_POINT('Ctrl Pts',(-0.307019775097118,-7.40030626975107,
-0.0208423447177452));
#11386=CARTESIAN_POINT('',(0.0795799710354742,-7.69739806084557,-1.93091915593928E-16));
#11387=CARTESIAN_POINT('Origin',(0.,-7.4,0.));
#11388=CARTESIAN_POINT('Ctrl Pts',(0.0795809081573368,-7.69740028961993,
2.49366499671666E-17));
#11389=CARTESIAN_POINT('Ctrl Pts',(-0.0133964972572649,-7.72194966690666,
-0.00499978774624427));
#11390=CARTESIAN_POINT('Ctrl Pts',(-0.21902209759443,-7.67864022412054,
-0.0147190061736624));
#11391=CARTESIAN_POINT('Ctrl Pts',(-0.307135787948618,-7.49066305702376,
-0.0244382246010806));
#11392=CARTESIAN_POINT('Ctrl Pts',(-0.307720604786163,-7.39984568899361,
-0.0291576552822545));
#11393=CARTESIAN_POINT('Origin',(0.,0.,0.));
#11394=CARTESIAN_POINT('',(-6.35,-7.77650717458569E-16,0.));
#11395=CARTESIAN_POINT('Origin',(0.,0.,0.));
#11396=CARTESIAN_POINT('',(-6.35,-7.77650717458569E-16,-0.2));
#11397=CARTESIAN_POINT('',(-6.35,7.77650717458569E-16,0.));
#11398=CARTESIAN_POINT('Origin',(0.,0.,-0.2));
#11399=CARTESIAN_POINT('Origin',(0.,0.,0.));
#11400=CARTESIAN_POINT('',(-6.85,-8.38883057415937E-16,0.));
#11401=CARTESIAN_POINT('Origin',(0.,0.,0.));
#11402=CARTESIAN_POINT('',(-6.85,-8.38883057415937E-16,-0.2));
#11403=CARTESIAN_POINT('',(-6.85,8.38883057415937E-16,0.));
#11404=CARTESIAN_POINT('Origin',(0.,0.,-0.2));
#11405=CARTESIAN_POINT('Origin',(0.,0.,-0.2));
#11406=CARTESIAN_POINT('Origin',(0.,0.,0.));
#11407=CARTESIAN_POINT('',(-1.68151315379565,-2.11246621596943,0.));
#11408=CARTESIAN_POINT('',(-2.7,-3.30654635769785E-16,0.));
#11409=CARTESIAN_POINT('Origin',(0.,0.,0.));
#11410=CARTESIAN_POINT('',(-1.68151315379564,2.11246621596944,0.));
#11411=CARTESIAN_POINT('Origin',(0.,0.,0.));
#11412=CARTESIAN_POINT('',(-1.37718656791819,1.58535710713571,1.11022302462516E-16));
#11413=CARTESIAN_POINT('',(-1.89641016151378,2.48467875173176,0.));
#11414=CARTESIAN_POINT('',(-1.37718656791819,-1.58535710713571,0.));
#11415=CARTESIAN_POINT('Origin',(0.,0.,0.));
#11416=CARTESIAN_POINT('',(-1.29641016151378,-1.44544826719043,0.));
#11417=CARTESIAN_POINT('',(-0.988692830768093,2.51246621596944,0.));
#11418=CARTESIAN_POINT('',(2.67020598456374,0.4,0.));
#11419=CARTESIAN_POINT('Origin',(0.,0.,0.));
#11420=CARTESIAN_POINT('',(2.06155281280883,0.4,0.));
#11421=CARTESIAN_POINT('',(3.1,0.4,0.));
#11422=CARTESIAN_POINT('',(-0.684366244890639,1.98535710713571,1.11022302462516E-16));
#11423=CARTESIAN_POINT('Origin',(0.,0.,0.));
#11424=CARTESIAN_POINT('',(-0.603589838486224,1.84544826719043,0.));
#11425=CARTESIAN_POINT('',(-0.988692830768095,-2.51246621596944,0.));
#11426=CARTESIAN_POINT('',(-0.684366244890641,-1.98535710713571,0.));
#11427=CARTESIAN_POINT('',(-1.20358983848623,-2.88467875173176,0.));
#11428=CARTESIAN_POINT('',(2.06155281280883,-0.4,0.));
#11429=CARTESIAN_POINT('Origin',(0.,0.,0.));
#11430=CARTESIAN_POINT('',(2.67020598456374,-0.4,0.));
#11431=CARTESIAN_POINT('',(1.9,-0.4,0.));
#11432=CARTESIAN_POINT('Origin',(0.,0.,0.));
#11433=CARTESIAN_POINT('',(-1.7,-2.0818995585505E-16,0.));
#11434=CARTESIAN_POINT('Origin',(0.,0.,0.));
#11435=CARTESIAN_POINT('Origin',(0.,-7.4,0.220842344717745));
#11436=CARTESIAN_POINT('Ctrl Pts',(-0.307720604786163,-7.39984568899361,
-0.0291576552822545));
#11437=CARTESIAN_POINT('Ctrl Pts',(-0.307784286494135,-7.38995643010364,
-0.0296715621794891));
#11438=CARTESIAN_POINT('Ctrl Pts',(-0.302900314845739,-7.27942155055893,
-0.0354188066551321));
#11439=CARTESIAN_POINT('Ctrl Pts',(-0.169525086729888,-7.08020524373302,
-0.0463993887091836));
#11440=CARTESIAN_POINT('Ctrl Pts',(0.1731988395346,-7.0822171223069,-0.0620994014444089));
#11441=CARTESIAN_POINT('Ctrl Pts',(0.360608974721706,-7.3691443808669,-0.0777994141796343));
#11442=CARTESIAN_POINT('Ctrl Pts',(0.224659927796838,-7.6837617716103,-0.0934994269148595));
#11443=CARTESIAN_POINT('Ctrl Pts',(-0.112744994253697,-7.74391654987674,
-0.109199439650085));
#11444=CARTESIAN_POINT('Ctrl Pts',(-0.291645305847843,-7.55598558781012,
-0.12108551577255));
#11445=CARTESIAN_POINT('Ctrl Pts',(-0.307476676298265,-7.42768934924628,
-0.127738254316606));
#11446=CARTESIAN_POINT('Ctrl Pts',(-0.307245641089215,-7.40026066578654,
-0.129157655282254));
#11447=CARTESIAN_POINT('Ctrl Pts',(-0.307019775097118,-7.40030626975107,
-0.0208423447177452));
#11448=CARTESIAN_POINT('Ctrl Pts',(-0.306554867615898,-7.33221201786739,
-0.0243615716353137));
#11449=CARTESIAN_POINT('Ctrl Pts',(-0.25102806371146,-7.16194939514258,
-0.0331141361312906));
#11450=CARTESIAN_POINT('Ctrl Pts',(0.0286357521188298,-7.03927813304723,
-0.047100038205676));
#11451=CARTESIAN_POINT('Ctrl Pts',(0.31666225793602,-7.22476085896309,-0.0628000509409014));
#11452=CARTESIAN_POINT('Ctrl Pts',(0.320850989126134,-7.56751742991046,
-0.0785000636761266));
#11453=CARTESIAN_POINT('Ctrl Pts',(0.0372719144191142,-7.75999252270946,
-0.0942000764113521));
#11454=CARTESIAN_POINT('Ctrl Pts',(-0.247682040721021,-7.64285422545096,
-0.108314170091892));
#11455=CARTESIAN_POINT('Ctrl Pts',(-0.306610223827363,-7.4702887152328,
-0.117194926194023));
#11456=CARTESIAN_POINT('Ctrl Pts',(-0.307159064170147,-7.39975436132604,
-0.120842344717745));
#11457=CARTESIAN_POINT('Ctrl Pts',(0.191346599666505,-7.2364012796625,0.));
#11458=CARTESIAN_POINT('Ctrl Pts',(0.245141179607852,-7.29931992554818,
-0.00523333757840845));
#11459=CARTESIAN_POINT('Ctrl Pts',(0.284951729745964,-7.48132135155768,
-0.0157000127352253));
#11460=CARTESIAN_POINT('Ctrl Pts',(0.0891127727595961,-7.6829132685142,
-0.0314000254704507));
#11461=CARTESIAN_POINT('Ctrl Pts',(-0.186694378247,-7.63020857787028,-0.047100038205676));
#11462=CARTESIAN_POINT('Ctrl Pts',(-0.295059602684748,-7.37136782429952,
-0.0628000509409014));
#11463=CARTESIAN_POINT('Ctrl Pts',(-0.138857786185943,-7.13805651573056,
-0.0785000636761267));
#11464=CARTESIAN_POINT('Ctrl Pts',(0.141866952506379,-7.13970444295027,
-0.0942000764113521));
#11465=CARTESIAN_POINT('Ctrl Pts',(0.295374359480038,-7.37472620101916,
-0.109900089146577));
#11466=CARTESIAN_POINT('Ctrl Pts',(0.184018665439577,-7.63242891167365,
-0.125600101881803));
#11467=CARTESIAN_POINT('Ctrl Pts',(-0.0923492835639111,-7.68170161519918,
-0.141300114617028));
#11468=CARTESIAN_POINT('Ctrl Pts',(-0.285906271942125,-7.47837412674206,
-0.157000127352253));
#11469=CARTESIAN_POINT('Ctrl Pts',(-0.223088597453814,-7.20476565095269,
-0.172700140087479));
#11470=CARTESIAN_POINT('Ctrl Pts',(0.0397748786158152,-7.10622675779884,
-0.188400152822704));
#11471=CARTESIAN_POINT('Ctrl Pts',(0.266971781925274,-7.2711166193684,-0.20410016555793));
#11472=CARTESIAN_POINT('Ctrl Pts',(0.254772555688239,-7.55157770749914,
-0.219800178293155));
#11473=CARTESIAN_POINT('Ctrl Pts',(0.0141163204507142,-7.69611748091033,
-0.23550019102838));
#11474=CARTESIAN_POINT('Ctrl Pts',(-0.239198147751981,-7.57512593293145,
-0.251200203763606));
#11475=CARTESIAN_POINT('Ctrl Pts',(-0.27802134557703,-7.29709724880236,
-0.266900216498831));
#11476=CARTESIAN_POINT('Ctrl Pts',(-0.0675401338845549,-7.11134246474494,
-0.282600229234056));
#11477=CARTESIAN_POINT('Ctrl Pts',(0.203504962958946,-7.18442965393879,
-0.298300241969281));
#11478=CARTESIAN_POINT('Ctrl Pts',(0.292065207602253,-7.45082084443414,
-0.314000254704507));
#11479=CARTESIAN_POINT('Ctrl Pts',(0.11872777843214,-7.67164049423864,-0.329700267439732));
#11480=CARTESIAN_POINT('Ctrl Pts',(-0.161073988577029,-7.64887750781731,
-0.345400280174958));
#11481=CARTESIAN_POINT('Ctrl Pts',(-0.296439164806322,-7.40294367203764,
-0.361100292910183));
#11482=CARTESIAN_POINT('Ctrl Pts',(-0.165984498020776,-7.15437021753843,
-0.376800305645409));
#11483=CARTESIAN_POINT('Ctrl Pts',(0.113310060512786,-7.12605534531845,
-0.392500318380633));
#11484=CARTESIAN_POINT('Ctrl Pts',(0.290998400738692,-7.34338927312074,
-0.408200331115859));
#11485=CARTESIAN_POINT('Ctrl Pts',(0.207745683316185,-7.61148658277481,
-0.423900343851084));
#11486=CARTESIAN_POINT('Ctrl Pts',(-0.0617945813750686,-7.68994184478043,
-0.439600356586309));
#11487=CARTESIAN_POINT('Ctrl Pts',(-0.275923052079717,-7.50840347294413,
-0.455300369321535));
#11488=CARTESIAN_POINT('Ctrl Pts',(-0.242628674974808,-7.22965866703555,
-0.47100038205676));
#11489=CARTESIAN_POINT('Ctrl Pts',(0.00823316280845383,-7.10366056839557,
-0.486700394791985));
#11490=CARTESIAN_POINT('Ctrl Pts',(0.251712244204393,-7.2433928813903,-0.502400407527211));
#11491=CARTESIAN_POINT('Ctrl Pts',(0.269478542032991,-7.52355629933161,
-0.518100420262436));
#11492=CARTESIAN_POINT('Ctrl Pts',(0.0456008446923772,-7.6929255997915,
-0.533800432997662));
#11493=CARTESIAN_POINT('Ctrl Pts',(-0.21916756500053,-7.59962570174306,
-0.549500445732887));
#11494=CARTESIAN_POINT('Ctrl Pts',(-0.287406321718959,-7.32731952781878,
-0.565200458468112));
#11495=CARTESIAN_POINT('Ctrl Pts',(-0.097925062092462,-7.12018661846282,
-0.580900471203338));
#11496=CARTESIAN_POINT('Ctrl Pts',(0.179366519168448,-7.16396507714928,
-0.596600483938563));
#11497=CARTESIAN_POINT('Ctrl Pts',(0.295818464274662,-7.41939826633471,
-0.612300496673789));
#11498=CARTESIAN_POINT('Ctrl Pts',(0.147007069090942,-7.65743694331754,
-0.628000509409014));
#11499=CARTESIAN_POINT('Ctrl Pts',(-0.13362680296465,-7.66462924315299,
-0.643700522144239));
#11500=CARTESIAN_POINT('Ctrl Pts',(-0.294436586401099,-7.43452636601645,
-0.659400534879464));
#11501=CARTESIAN_POINT('Ctrl Pts',(-0.191221557053218,-7.17346255012345,
-0.675100547614691));
#11502=CARTESIAN_POINT('Ctrl Pts',(0.0834622628790381,-7.11553868302403,
-0.690800560349915));
#11503=CARTESIAN_POINT('Ctrl Pts',(0.28330752343249,-7.31269069134103,-0.706500573085141));
#11504=CARTESIAN_POINT('Ctrl Pts',(0.229102456085247,-7.58814048413055,
-0.722200585820366));
#11505=CARTESIAN_POINT('Ctrl Pts',(-0.0305293756465861,-7.6948694057645,
-0.737900598555591));
#11506=CARTESIAN_POINT('Ctrl Pts',(-0.26280863385947,-7.53721332189184,
-0.753600611290817));
#11507=CARTESIAN_POINT('Ctrl Pts',(-0.25937764590646,-7.25646182589342,
-0.769300624026042));
#11508=CARTESIAN_POINT('Ctrl Pts',(-0.0234555070157643,-7.10453321779813,
-0.785000636761267));
#11509=CARTESIAN_POINT('Ctrl Pts',(0.233691827601142,-7.21732779772848,
-0.800700649496493));
#11510=CARTESIAN_POINT('Ctrl Pts',(0.280893064283751,-7.49439140290128,
-0.816400662231719));
#11511=CARTESIAN_POINT('Ctrl Pts',(0.144991950449976,-7.62182878450703,
-0.826867337388535));
#11512=CARTESIAN_POINT('Ctrl Pts',(0.0650199997975086,-7.64320868020351,
-0.832100674966944));
#11513=CARTESIAN_POINT('Ctrl Pts',(0.205433155034208,-7.22435746787732,
0.0107002249889811));
#11514=CARTESIAN_POINT('Ctrl Pts',(0.263187984753429,-7.291908059094,0.00546688741057261));
#11515=CARTESIAN_POINT('Ctrl Pts',(0.305929308261523,-7.48730806740887,
-0.00499978774624425));
#11516=CARTESIAN_POINT('Ctrl Pts',(0.0956730775135631,-7.70374077957594,
-0.0206998004814697));
#11517=CARTESIAN_POINT('Ctrl Pts',(-0.200438446344363,-7.64715607463241,
-0.0363998132166949));
#11518=CARTESIAN_POINT('Ctrl Pts',(-0.316781302663923,-7.36925998058027,
-0.0520998259519204));
#11519=CARTESIAN_POINT('Ctrl Pts',(-0.149080219700592,-7.11877275839805,
-0.0677998386871456));
#11520=CARTESIAN_POINT('Ctrl Pts',(0.152310914849119,-7.12054200273581,
-0.0834998514223711));
#11521=CARTESIAN_POINT('Ctrl Pts',(0.31711923122726,-7.37286559430175,-0.0991998641575963));
#11522=CARTESIAN_POINT('Ctrl Pts',(0.197565752891998,-7.64953986498586,
-0.114899876892822));
#11523=CARTESIAN_POINT('Ctrl Pts',(-0.0991478537938397,-7.70243992675837,
-0.130599889628047));
#11524=CARTESIAN_POINT('Ctrl Pts',(-0.306954121952032,-7.48414387377529,
-0.146299902363272));
#11525=CARTESIAN_POINT('Ctrl Pts',(-0.23951193544578,-7.19039288722277,
-0.161999915098498));
#11526=CARTESIAN_POINT('Ctrl Pts',(0.0427030259194093,-7.08459975711512,
-0.177699927833723));
#11527=CARTESIAN_POINT('Ctrl Pts',(0.286625712511232,-7.26162848171449,
-0.193399940568948));
#11528=CARTESIAN_POINT('Ctrl Pts',(0.273528403548241,-7.56273655627365,
-0.209099953304174));
#11529=CARTESIAN_POINT('Ctrl Pts',(0.0151555358324549,-7.71791705977642,
-0.224799966039399));
#11530=CARTESIAN_POINT('Ctrl Pts',(-0.256807438735113,-7.58801835513732,
-0.240499978774624));
#11531=CARTESIAN_POINT('Ctrl Pts',(-0.29848872302037,-7.28952175331532,
-0.25619999150985));
#11532=CARTESIAN_POINT('Ctrl Pts',(-0.0725123039527193,-7.09009207221242,
-0.271900004245075));
#11533=CARTESIAN_POINT('Ctrl Pts',(0.218486592804054,-7.1685597946326,-0.287600016980301));
#11534=CARTESIAN_POINT('Ctrl Pts',(0.313566466182439,-7.45456217372979,
-0.303300029715526));
#11535=CARTESIAN_POINT('Ctrl Pts',(0.127468280889375,-7.69163812612169,
-0.319000042450751));
#11536=CARTESIAN_POINT('Ctrl Pts',(-0.172931934641091,-7.66719937400022,
-0.334700055185977));
#11537=CARTESIAN_POINT('Ctrl Pts',(-0.31826242539981,-7.40316037930715,
-0.350400067921202));
#11538=CARTESIAN_POINT('Ctrl Pts',(-0.178203946004828,-7.13628744242441,
-0.366100080656428));
#11539=CARTESIAN_POINT('Ctrl Pts',(0.12165172137278,-7.10588808573515,-0.381800093391652));
#11540=CARTESIAN_POINT('Ctrl Pts',(0.312421123123427,-7.33922170421708,
-0.397500106126878));
#11541=CARTESIAN_POINT('Ctrl Pts',(0.223039506543434,-7.62705580356564,
-0.413200118862103));
#11542=CARTESIAN_POINT('Ctrl Pts',(-0.0663437753167488,-7.71128678562093,
-0.428900131597329));
#11543=CARTESIAN_POINT('Ctrl Pts',(-0.296235957337091,-7.51638392060476,
-0.444600144332554));
#11544=CARTESIAN_POINT('Ctrl Pts',(-0.260490514536012,-7.21711847754488,
-0.460300157067779));
#11545=CARTESIAN_POINT('Ctrl Pts',(0.0088392718480435,-7.08184464996167,
-0.476000169803005));
#11546=CARTESIAN_POINT('Ctrl Pts',(0.27024279803129,-7.23186377739202,-0.49170018253823));
#11547=CARTESIAN_POINT('Ctrl Pts',(0.289317015302814,-7.53265226787559,
-0.507400195273456));
#11548=CARTESIAN_POINT('Ctrl Pts',(0.0489578880090222,-7.71449019873013,
-0.52310020800868));
#11549=CARTESIAN_POINT('Ctrl Pts',(-0.235302244396795,-7.61432174810773,
-0.538800220743907));
#11550=CARTESIAN_POINT('Ctrl Pts',(-0.308564602404261,-7.32196893628847,
-0.554500233479131));
#11551=CARTESIAN_POINT('Ctrl Pts',(-0.10513411002671,-7.0995873149031,-0.570200246214357));
#11552=CARTESIAN_POINT('Ctrl Pts',(0.192571124882802,-7.14658865647997,
-0.585900258949582));
#11553=CARTESIAN_POINT('Ctrl Pts',(0.317596030131889,-7.42082632804701,
-0.601600271684808));
#11554=CARTESIAN_POINT('Ctrl Pts',(0.157829436573836,-7.67638893808543,
-0.617300284420033));
#11555=CARTESIAN_POINT('Ctrl Pts',(-0.14346414191842,-7.68411072070256,
-0.633000297155258));
#11556=CARTESIAN_POINT('Ctrl Pts',(-0.316112421162968,-7.43706812828128,
-0.648700309890484));
#11557=CARTESIAN_POINT('Ctrl Pts',(-0.205298907032905,-7.15678531448872,
-0.664400322625708));
#11558=CARTESIAN_POINT('Ctrl Pts',(0.0896065883554691,-7.09459720771934,
-0.680100335360935));
#11559=CARTESIAN_POINT('Ctrl Pts',(0.30416405875569,-7.30626315402036,-0.69580034809616));
#11560=CARTESIAN_POINT('Ctrl Pts',(0.245968522365736,-7.60199101166138,
-0.711500360831385));
#11561=CARTESIAN_POINT('Ctrl Pts',(-0.0327768874452623,-7.71657710382541,
-0.72720037356661));
#11562=CARTESIAN_POINT('Ctrl Pts',(-0.282156081780803,-7.54731469322211,
-0.742900386301835));
#11563=CARTESIAN_POINT('Ctrl Pts',(-0.278472511331682,-7.24589483154675,
-0.758600399037061));
#11564=CARTESIAN_POINT('Ctrl Pts',(-0.025182254702062,-7.0827815420743,
-0.774300411772286));
#11565=CARTESIAN_POINT('Ctrl Pts',(0.25089575426731,-7.20387983421137,-0.790000424507512));
#11566=CARTESIAN_POINT('Ctrl Pts',(0.301571851935755,-7.50134030988745,
-0.805700437242737));
#11567=CARTESIAN_POINT('Ctrl Pts',(0.155665968914086,-7.6381593775803,-0.816167112399554));
#11568=CARTESIAN_POINT('Ctrl Pts',(0.0698066426161003,-7.66111321859386,
-0.821400449977962));
#11569=CARTESIAN_POINT('Ctrl Pts',(0.219519710401911,-7.21231365609212,
0.0214004499779621));
#11570=CARTESIAN_POINT('Ctrl Pts',(0.281234789899005,-7.28449619263982,
0.0161671123995537));
#11571=CARTESIAN_POINT('Ctrl Pts',(0.326906886777081,-7.49329478326005,
0.0057004372427368));
#11572=CARTESIAN_POINT('Ctrl Pts',(0.10223338226753,-7.7245682906377,-0.00999957549248859));
#11573=CARTESIAN_POINT('Ctrl Pts',(-0.214182514441725,-7.66410357139452,
-0.0256995882277139));
#11574=CARTESIAN_POINT('Ctrl Pts',(-0.338503002643098,-7.36715213686105,
-0.0413996009629393));
#11575=CARTESIAN_POINT('Ctrl Pts',(-0.15930265321524,-7.09948900106554,
-0.0570996136981646));
#11576=CARTESIAN_POINT('Ctrl Pts',(0.162754877191859,-7.10137956252136,
-0.07279962643339));
#11577=CARTESIAN_POINT('Ctrl Pts',(0.338864102974484,-7.37100498758432,
-0.0884996391686153));
#11578=CARTESIAN_POINT('Ctrl Pts',(0.211112840344417,-7.66665081829808,
-0.104199651903841));
#11579=CARTESIAN_POINT('Ctrl Pts',(-0.105946424023768,-7.72317823831756,
-0.119899664639066));
#11580=CARTESIAN_POINT('Ctrl Pts',(-0.328001971961939,-7.48991362080854,
-0.135599677374291));
#11581=CARTESIAN_POINT('Ctrl Pts',(-0.255935273437745,-7.17602012349283,
-0.151299690109517));
#11582=CARTESIAN_POINT('Ctrl Pts',(0.0456311732230033,-7.06297275643139,
-0.166999702844742));
#11583=CARTESIAN_POINT('Ctrl Pts',(0.306279643097191,-7.25214034406058,
-0.182699715579967));
#11584=CARTESIAN_POINT('Ctrl Pts',(0.292284251408242,-7.57389540504817,
-0.198399728315193));
#11585=CARTESIAN_POINT('Ctrl Pts',(0.0161947512141955,-7.7397166386425,
-0.214099741050418));
#11586=CARTESIAN_POINT('Ctrl Pts',(-0.274416729718245,-7.60091077734321,
-0.229799753785643));
#11587=CARTESIAN_POINT('Ctrl Pts',(-0.31895610046371,-7.28194625782827,
-0.245499766520869));
#11588=CARTESIAN_POINT('Ctrl Pts',(-0.0774844740208837,-7.06884167967991,
-0.261199779256094));
#11589=CARTESIAN_POINT('Ctrl Pts',(0.233468222649161,-7.15268993532641,
-0.27689979199132));
#11590=CARTESIAN_POINT('Ctrl Pts',(0.335067724762625,-7.45830350302544,
-0.292599804726544));
#11591=CARTESIAN_POINT('Ctrl Pts',(0.13620878334661,-7.71163575800473,-0.308299817461771));
#11592=CARTESIAN_POINT('Ctrl Pts',(-0.184789880705154,-7.68552124018313,
-0.323999830196995));
#11593=CARTESIAN_POINT('Ctrl Pts',(-0.340085685993297,-7.40337708657666,
-0.339699842932221));
#11594=CARTESIAN_POINT('Ctrl Pts',(-0.19042339398888,-7.11820466731038,
-0.355399855667446));
#11595=CARTESIAN_POINT('Ctrl Pts',(0.129993382232775,-7.08572082615184,
-0.371099868402671));
#11596=CARTESIAN_POINT('Ctrl Pts',(0.333843845508162,-7.33505413531342,
-0.386799881137897));
#11597=CARTESIAN_POINT('Ctrl Pts',(0.238333329770683,-7.64262502435649,
-0.402499893873123));
#11598=CARTESIAN_POINT('Ctrl Pts',(-0.070892969258429,-7.73263172646143,
-0.418199906608347));
#11599=CARTESIAN_POINT('Ctrl Pts',(-0.316548862594466,-7.52436436826539,
-0.433899919343574));
#11600=CARTESIAN_POINT('Ctrl Pts',(-0.278352354097216,-7.20457828805423,
-0.449599932078798));
#11601=CARTESIAN_POINT('Ctrl Pts',(0.00944538088763332,-7.06002873152775,
-0.465299944814024));
#11602=CARTESIAN_POINT('Ctrl Pts',(0.288773351858187,-7.22033467339375,
-0.480999957549248));
#11603=CARTESIAN_POINT('Ctrl Pts',(0.309155488572638,-7.54174823641955,
-0.496699970284475));
#11604=CARTESIAN_POINT('Ctrl Pts',(0.052314931325667,-7.73605479766878,
-0.512399983019699));
#11605=CARTESIAN_POINT('Ctrl Pts',(-0.251436923793061,-7.62901779447239,
-0.528099995754926));
#11606=CARTESIAN_POINT('Ctrl Pts',(-0.329722883089562,-7.31661834475815,
-0.54380000849015));
#11607=CARTESIAN_POINT('Ctrl Pts',(-0.112343157960958,-7.0789880113434,
-0.559500021225376));
#11608=CARTESIAN_POINT('Ctrl Pts',(0.205775730597156,-7.12921223581066,
-0.575200033960601));
#11609=CARTESIAN_POINT('Ctrl Pts',(0.339373595989117,-7.4222543897593,-0.590900046695826));
#11610=CARTESIAN_POINT('Ctrl Pts',(0.168651804056731,-7.69534093285333,
-0.606600059431053));
#11611=CARTESIAN_POINT('Ctrl Pts',(-0.15330148087219,-7.70359219825212,
-0.622300072166277));
#11612=CARTESIAN_POINT('Ctrl Pts',(-0.337788255924836,-7.43960989054611,
-0.638000084901503));
#11613=CARTESIAN_POINT('Ctrl Pts',(-0.219376257012592,-7.14010807885398,
-0.653700097636727));
#11614=CARTESIAN_POINT('Ctrl Pts',(0.0957509138319004,-7.07365573241465,
-0.669400110371954));
#11615=CARTESIAN_POINT('Ctrl Pts',(0.325020594078889,-7.29983561669969,
-0.685100123107178));
#11616=CARTESIAN_POINT('Ctrl Pts',(0.262834588646226,-7.6158415391922,-0.700800135842404));
#11617=CARTESIAN_POINT('Ctrl Pts',(-0.0350243992439388,-7.73828480188633,
-0.716500148577629));
#11618=CARTESIAN_POINT('Ctrl Pts',(-0.301503529702136,-7.55741606455238,
-0.732200161312854));
#11619=CARTESIAN_POINT('Ctrl Pts',(-0.297567376756904,-7.23532783720007,
-0.74790017404808));
#11620=CARTESIAN_POINT('Ctrl Pts',(-0.0269090023883596,-7.06102986635047,
-0.763600186783306));
#11621=CARTESIAN_POINT('Ctrl Pts',(0.268099680933479,-7.19043187069426,
-0.77930019951853));
#11622=CARTESIAN_POINT('Ctrl Pts',(0.32225063958776,-7.50828921687363,-0.795000212253757));
#11623=CARTESIAN_POINT('Ctrl Pts',(0.166339987378195,-7.65448997065358,
-0.805466887410573));
#11624=CARTESIAN_POINT('Ctrl Pts',(0.074593285434692,-7.67901775698422,
-0.810700224988981));
#11625=CARTESIAN_POINT('Ctrl Pts',(0.233606265769614,-7.20026984430693,
0.0321006749669432));
#11626=CARTESIAN_POINT('Ctrl Pts',(0.299281595044582,-7.27708432618563,
0.0268673373885347));
#11627=CARTESIAN_POINT('Ctrl Pts',(0.34788446529264,-7.49928149911123,0.0164006622317179));
#11628=CARTESIAN_POINT('Ctrl Pts',(0.108793687021496,-7.74539580169946,
0.000700649496492485));
#11629=CARTESIAN_POINT('Ctrl Pts',(-0.227926582539088,-7.68105106815663,
-0.0149993632387328));
#11630=CARTESIAN_POINT('Ctrl Pts',(-0.360224702622273,-7.36504429314182,
-0.0306993759739582));
#11631=CARTESIAN_POINT('Ctrl Pts',(-0.169525086729888,-7.08020524373302,
-0.0463993887091836));
#11632=CARTESIAN_POINT('Ctrl Pts',(0.1731988395346,-7.0822171223069,-0.0620994014444089));
#11633=CARTESIAN_POINT('Ctrl Pts',(0.360608974721706,-7.3691443808669,-0.0777994141796343));
#11634=CARTESIAN_POINT('Ctrl Pts',(0.224659927796838,-7.6837617716103,-0.0934994269148595));
#11635=CARTESIAN_POINT('Ctrl Pts',(-0.112744994253697,-7.74391654987674,
-0.109199439650085));
#11636=CARTESIAN_POINT('Ctrl Pts',(-0.349049821971846,-7.49568336784179,
-0.12489945238531));
#11637=CARTESIAN_POINT('Ctrl Pts',(-0.272358611429711,-7.16164735976291,
-0.140599465120536));
#11638=CARTESIAN_POINT('Ctrl Pts',(0.0485593205265976,-7.04134575574766,
-0.156299477855761));
#11639=CARTESIAN_POINT('Ctrl Pts',(0.32593357368315,-7.24265220640667,-0.171999490590986));
#11640=CARTESIAN_POINT('Ctrl Pts',(0.311040099268243,-7.58505425382268,
-0.187699503326212));
#11641=CARTESIAN_POINT('Ctrl Pts',(0.017233966595936,-7.7615162175086,-0.203399516061437));
#11642=CARTESIAN_POINT('Ctrl Pts',(-0.292026020701376,-7.61380319954907,
-0.219099528796662));
#11643=CARTESIAN_POINT('Ctrl Pts',(-0.339423477907051,-7.27437076234124,
-0.234799541531888));
#11644=CARTESIAN_POINT('Ctrl Pts',(-0.0824566440890477,-7.04759128714739,
-0.250499554267113));
#11645=CARTESIAN_POINT('Ctrl Pts',(0.248449852494269,-7.13682007602022,
-0.266199567002339));
#11646=CARTESIAN_POINT('Ctrl Pts',(0.356568983342811,-7.46204483232109,
-0.281899579737564));
#11647=CARTESIAN_POINT('Ctrl Pts',(0.144949285803845,-7.73163338988777,
-0.297599592472789));
#11648=CARTESIAN_POINT('Ctrl Pts',(-0.196647826769216,-7.70384310636604,
-0.313299605208015));
#11649=CARTESIAN_POINT('Ctrl Pts',(-0.361908946586785,-7.40359379384616,
-0.32899961794324));
#11650=CARTESIAN_POINT('Ctrl Pts',(-0.202642841972932,-7.10012189219636,
-0.344699630678465));
#11651=CARTESIAN_POINT('Ctrl Pts',(0.13833504309277,-7.06555356656853,-0.36039964341369));
#11652=CARTESIAN_POINT('Ctrl Pts',(0.355266567892898,-7.33088656640977,
-0.376099656148916));
#11653=CARTESIAN_POINT('Ctrl Pts',(0.253627152997932,-7.65819424514732,
-0.391799668884141));
#11654=CARTESIAN_POINT('Ctrl Pts',(-0.0754421632001089,-7.75397666730194,
-0.407499681619367));
#11655=CARTESIAN_POINT('Ctrl Pts',(-0.336861767851841,-7.53234481592602,
-0.423199694354592));
#11656=CARTESIAN_POINT('Ctrl Pts',(-0.29621419365842,-7.19203809856356,
-0.438899707089817));
#11657=CARTESIAN_POINT('Ctrl Pts',(0.010051489927223,-7.03821281309385,
-0.454599719825043));
#11658=CARTESIAN_POINT('Ctrl Pts',(0.307303905685085,-7.20880556939548,
-0.470299732560268));
#11659=CARTESIAN_POINT('Ctrl Pts',(0.328993961842462,-7.55084420496352,
-0.485999745295494));
#11660=CARTESIAN_POINT('Ctrl Pts',(0.0556719746423119,-7.75761939660742,
-0.501699758030718));
#11661=CARTESIAN_POINT('Ctrl Pts',(-0.267571603189326,-7.64371384083705,
-0.517399770765944));
#11662=CARTESIAN_POINT('Ctrl Pts',(-0.350881163774864,-7.31126775322783,
-0.533099783501169));
#11663=CARTESIAN_POINT('Ctrl Pts',(-0.119552205895206,-7.05838870778368,
-0.548799796236395));
#11664=CARTESIAN_POINT('Ctrl Pts',(0.21898033631151,-7.11183581514136,-0.56449980897162));
#11665=CARTESIAN_POINT('Ctrl Pts',(0.361151161846345,-7.42368245147158,
-0.580199821706845));
#11666=CARTESIAN_POINT('Ctrl Pts',(0.179474171539626,-7.71429292762124,
-0.595899834442071));
#11667=CARTESIAN_POINT('Ctrl Pts',(-0.16313881982596,-7.72307367580168,
-0.611599847177296));
#11668=CARTESIAN_POINT('Ctrl Pts',(-0.359464090686704,-7.44215165281094,
-0.627299859912522));
#11669=CARTESIAN_POINT('Ctrl Pts',(-0.23345360699228,-7.12343084321925,
-0.642999872647746));
#11670=CARTESIAN_POINT('Ctrl Pts',(0.101895239308332,-7.05271425710996,
-0.658699885382973));
#11671=CARTESIAN_POINT('Ctrl Pts',(0.345877129402089,-7.29340807937902,
-0.674399898118197));
#11672=CARTESIAN_POINT('Ctrl Pts',(0.279700654926715,-7.62969206672302,
-0.690099910853423));
#11673=CARTESIAN_POINT('Ctrl Pts',(-0.0372719110426151,-7.75999249994725,
-0.705799923588648));
#11674=CARTESIAN_POINT('Ctrl Pts',(-0.320850977623468,-7.56751743588265,
-0.721499936323874));
#11675=CARTESIAN_POINT('Ctrl Pts',(-0.316662242182126,-7.2247608428534,
-0.7371999490591));
#11676=CARTESIAN_POINT('Ctrl Pts',(-0.0286357500746574,-7.03927819062664,
-0.752899961794323));
#11677=CARTESIAN_POINT('Ctrl Pts',(0.285303607599647,-7.17698390717715,
-0.76859997452955));
#11678=CARTESIAN_POINT('Ctrl Pts',(0.342929427239765,-7.51523812385981,
-0.784299987264775));
#11679=CARTESIAN_POINT('Ctrl Pts',(0.177014005842305,-7.67082056372685,
-0.794766662421592));
#11680=CARTESIAN_POINT('Ctrl Pts',(0.0793799282532836,-7.69692229537457,
-0.8));
#11681=CARTESIAN_POINT('Ctrl Pts',(0.0793799282532837,-7.69692229537457,
-0.8));
#11682=CARTESIAN_POINT('Ctrl Pts',(0.0961911535774395,-7.69077267405574,
-0.8));
#11683=CARTESIAN_POINT('Ctrl Pts',(0.112330843922834,-7.68307124108963,
-0.800000000000001));
#11684=CARTESIAN_POINT('Ctrl Pts',(0.127669392025775,-7.67400023114597,
-0.800000000000001));
#11685=CARTESIAN_POINT('Ctrl Pts',(0.137645102295363,-7.66810073098187,
-0.8));
#11686=CARTESIAN_POINT('Ctrl Pts',(0.147281499905208,-7.66162083360303,
-0.8));
#11687=CARTESIAN_POINT('Ctrl Pts',(0.156535308745364,-7.65460204840892,
-0.8));
#11688=CARTESIAN_POINT('Ctrl Pts',(0.16394907438502,-7.6489788904852,-0.8));
#11689=CARTESIAN_POINT('Ctrl Pts',(0.171117175854576,-7.64300969246698,
-0.8));
#11690=CARTESIAN_POINT('Ctrl Pts',(0.178013695811224,-7.63671383667496,
-0.8));
#11691=CARTESIAN_POINT('Ctrl Pts',(0.181540623741549,-7.63349409254636,
-0.8));
#11692=CARTESIAN_POINT('Ctrl Pts',(0.18499019303302,-7.63019453557326,-0.8));
#11693=CARTESIAN_POINT('Ctrl Pts',(0.188356686614326,-7.62682145400554,
-0.8));
#11694=CARTESIAN_POINT('Ctrl Pts',(0.200715909300271,-7.61443804520746,
-0.8));
#11695=CARTESIAN_POINT('Ctrl Pts',(0.2119727366568,-7.60105296662967,-0.8));
#11696=CARTESIAN_POINT('Ctrl Pts',(0.221976954632972,-7.58681403533943,
-0.8));
#11697=CARTESIAN_POINT('Ctrl Pts',(0.228265905107983,-7.57786301748729,
-0.8));
#11698=CARTESIAN_POINT('Ctrl Pts',(0.234059046958926,-7.56857397550235,
-0.800000000000001));
#11699=CARTESIAN_POINT('Ctrl Pts',(0.239308880691954,-7.55898034246681,
-0.800000000000001));
#11700=CARTESIAN_POINT('Ctrl Pts',(0.241553642901407,-7.55487822685998,
-0.800000000000001));
#11701=CARTESIAN_POINT('Ctrl Pts',(0.243698962884783,-7.55072040648099,
-0.8));
#11702=CARTESIAN_POINT('Ctrl Pts',(0.245740613533059,-7.54650946019889,
-0.8));
#11703=CARTESIAN_POINT('Ctrl Pts',(0.247686929038575,-7.54249514460152,
-0.8));
#11704=CARTESIAN_POINT('Ctrl Pts',(0.249535114515858,-7.53844054532369,
-0.8));
#11705=CARTESIAN_POINT('Ctrl Pts',(0.251281773031569,-7.53435014256214,
-0.8));
#11706=CARTESIAN_POINT('Ctrl Pts',(0.25753761623788,-7.51969993011548,-0.8));
#11707=CARTESIAN_POINT('Ctrl Pts',(0.262498419038268,-7.50458280996037,
-0.800000000000001));
#11708=CARTESIAN_POINT('Ctrl Pts',(0.266024763128534,-7.48910875296159,
-0.800000000000001));
#11709=CARTESIAN_POINT('Ctrl Pts',(0.268541680001999,-7.47806419401775,
-0.8));
#11710=CARTESIAN_POINT('Ctrl Pts',(0.270326758003547,-7.46683739589159,
-0.8));
#11711=CARTESIAN_POINT('Ctrl Pts',(0.271391872668289,-7.45549714829965,
-0.800000000000001));
#11712=CARTESIAN_POINT('Ctrl Pts',(0.27180519341859,-7.45109653323119,-0.800000000000001));
#11713=CARTESIAN_POINT('Ctrl Pts',(0.272109991496476,-7.44667886409003,
-0.8));
#11714=CARTESIAN_POINT('Ctrl Pts',(0.272306569544964,-7.4422483195902,-0.8));
#11715=CARTESIAN_POINT('Ctrl Pts',(0.272509069569706,-7.43768430352772,
-0.8));
#11716=CARTESIAN_POINT('Ctrl Pts',(0.272596269292494,-7.43311641885229,
-0.8));
#11717=CARTESIAN_POINT('Ctrl Pts',(0.272569843180126,-7.42855121408732,
-0.8));
#11718=CARTESIAN_POINT('Ctrl Pts',(0.272471763334016,-7.41160757233752,
-0.8));
#11719=CARTESIAN_POINT('Ctrl Pts',(0.270813105492815,-7.3946899321374,-0.8));
#11720=CARTESIAN_POINT('Ctrl Pts',(0.267648469785739,-7.37802931988141,
-0.8));
#11721=CARTESIAN_POINT('Ctrl Pts',(0.265994340517827,-7.36932095376763,
-0.8));
#11722=CARTESIAN_POINT('Ctrl Pts',(0.263927860253695,-7.36068304066339,
-0.8));
#11723=CARTESIAN_POINT('Ctrl Pts',(0.261451436850857,-7.35215158032667,
-0.8));
#11724=CARTESIAN_POINT('Ctrl Pts',(0.26000111795531,-7.34715512531064,-0.8));
#11725=CARTESIAN_POINT('Ctrl Pts',(0.258409538895798,-7.34219357239197,
-0.8));
#11726=CARTESIAN_POINT('Ctrl Pts',(0.256678528275944,-7.33727990943004,
-0.8));
#11727=CARTESIAN_POINT('Ctrl Pts',(0.251357982528078,-7.32217695842633,
-0.8));
#11728=CARTESIAN_POINT('Ctrl Pts',(0.244748768101333,-7.30759386618852,
-0.8));
#11729=CARTESIAN_POINT('Ctrl Pts',(0.236874461322484,-7.2937452086627,-0.8));
#11730=CARTESIAN_POINT('Ctrl Pts',(0.232807858999536,-7.28659321618312,
-0.8));
#11731=CARTESIAN_POINT('Ctrl Pts',(0.228399170212801,-7.27963280000633,
-0.8));
#11732=CARTESIAN_POINT('Ctrl Pts',(0.223669087593591,-7.27292514292032,
-0.8));
#11733=CARTESIAN_POINT('Ctrl Pts',(0.21642296268428,-7.26264952513373,-0.8));
#11734=CARTESIAN_POINT('Ctrl Pts',(0.208418195009514,-7.25295420792725,
-0.8));
#11735=CARTESIAN_POINT('Ctrl Pts',(0.199658648264246,-7.24395737393901,
-0.8));
#11736=CARTESIAN_POINT('Ctrl Pts',(0.197072110678764,-7.24130076967196,
-0.8));
#11737=CARTESIAN_POINT('Ctrl Pts',(0.194419670008508,-7.23870520686924,
-0.8));
#11738=CARTESIAN_POINT('Ctrl Pts',(0.191704041017359,-7.23617187252307,
-0.8));
#11739=CARTESIAN_POINT('Ctrl Pts',(0.191346599666505,-7.2364012796625,0.));
#11740=CARTESIAN_POINT('Ctrl Pts',(0.202509817473759,-7.24689196324677,
-4.25187765113737E-19));
#11741=CARTESIAN_POINT('Ctrl Pts',(0.212570029866005,-7.25841325449013,
1.70283439359328E-17));
#11742=CARTESIAN_POINT('Ctrl Pts',(0.221522302700304,-7.27074765126196,
1.73472347597681E-17));
#11743=CARTESIAN_POINT('Ctrl Pts',(0.229528851253605,-7.28177903384573,
1.76324377368777E-17));
#11744=CARTESIAN_POINT('Ctrl Pts',(0.236649204955062,-7.29346212976217,
-1.68985376951836E-17));
#11745=CARTESIAN_POINT('Ctrl Pts',(0.242860412371513,-7.30566884695974,
1.73472347597681E-18));
#11746=CARTESIAN_POINT('Ctrl Pts',(0.244940798159157,-7.30975737263099,
7.97575989914875E-18));
#11747=CARTESIAN_POINT('Ctrl Pts',(0.246919671013813,-7.31390628918125,
1.8683266199719E-17));
#11748=CARTESIAN_POINT('Ctrl Pts',(0.248793544918815,-7.31810659182485,
2.08166817117217E-17));
#11749=CARTESIAN_POINT('Ctrl Pts',(0.255493762728008,-7.33312518112348,
2.84449156978875E-17));
#11750=CARTESIAN_POINT('Ctrl Pts',(0.260811093553058,-7.34869786677283,
7.65141509275329E-17));
#11751=CARTESIAN_POINT('Ctrl Pts',(0.264722827386125,-7.36459856759787,
5.89805981832114E-17));
#11752=CARTESIAN_POINT('Ctrl Pts',(0.267427565046703,-7.37559298239867,
4.68571607370262E-17));
#11753=CARTESIAN_POINT('Ctrl Pts',(0.269459624700383,-7.38674528662227,
4.0452509126737E-17));
#11754=CARTESIAN_POINT('Ctrl Pts',(0.270799674072059,-7.39798906439888,
4.16333634234434E-17));
#11755=CARTESIAN_POINT('Ctrl Pts',(0.271554626847406,-7.40432354834945,
4.22986293811185E-17));
#11756=CARTESIAN_POINT('Ctrl Pts',(0.27208975223859,-7.41068715911504,6.88910133647342E-17));
#11757=CARTESIAN_POINT('Ctrl Pts',(0.272399999297887,-7.41706844790294,
6.59194920871187E-17));
#11758=CARTESIAN_POINT('Ctrl Pts',(0.272610263460686,-7.4213932474598,6.39055989172972E-17));
#11759=CARTESIAN_POINT('Ctrl Pts',(0.272716738029981,-7.42571709930175,
-1.06875105497055E-17));
#11760=CARTESIAN_POINT('Ctrl Pts',(0.272718929390231,-7.43003454190223,
-8.67361737988404E-18));
#11761=CARTESIAN_POINT('Ctrl Pts',(0.272726931468211,-7.44580032589523,
-1.31958684872211E-18));
#11762=CARTESIAN_POINT('Ctrl Pts',(0.27134758489836,-7.46148679133341,5.78590717144025E-17));
#11763=CARTESIAN_POINT('Ctrl Pts',(0.268538129113132,-7.47691813343808,
5.20417042793042E-17));
#11764=CARTESIAN_POINT('Ctrl Pts',(0.266219645760504,-7.4896527384696,4.04832294204731E-17));
#11765=CARTESIAN_POINT('Ctrl Pts',(0.262926744086474,-7.50221429697178,
3.27839278289332E-17));
#11766=CARTESIAN_POINT('Ctrl Pts',(0.258732626744963,-7.51453551399731,
4.5102810375397E-17));
#11767=CARTESIAN_POINT('Ctrl Pts',(0.256787792726102,-7.52024892639706,
5.08151402650737E-17));
#11768=CARTESIAN_POINT('Ctrl Pts',(0.254646875440068,-7.52591460238169,
4.71189268070476E-17));
#11769=CARTESIAN_POINT('Ctrl Pts',(0.252327893343031,-7.5314990454491,4.5102810375397E-17));
#11770=CARTESIAN_POINT('Ctrl Pts',(0.245813460854531,-7.54718673764602,
3.94391813203355E-17));
#11771=CARTESIAN_POINT('Ctrl Pts',(0.237886907768047,-7.56227236975653,
3.73105788674031E-17));
#11772=CARTESIAN_POINT('Ctrl Pts',(0.228725878996942,-7.5766134557043,1.04083408558608E-17));
#11773=CARTESIAN_POINT('Ctrl Pts',(0.223374521430301,-7.58499071121981,
-5.30643294735275E-18));
#11774=CARTESIAN_POINT('Ctrl Pts',(0.217600893833204,-7.59311391451407,
3.69689762542118E-17));
#11775=CARTESIAN_POINT('Ctrl Pts',(0.211432791129273,-7.60095290540197,
3.46944695195361E-17));
#11776=CARTESIAN_POINT('Ctrl Pts',(0.207420148579369,-7.60605253974577,
3.32147953082452E-17));
#11777=CARTESIAN_POINT('Ctrl Pts',(0.20324045059128,-7.61103185738154,2.54856801722722E-17));
#11778=CARTESIAN_POINT('Ctrl Pts',(0.198900278349408,-7.61588193104767,
3.12250225675825E-17));
#11779=CARTESIAN_POINT('Ctrl Pts',(0.195670728628085,-7.61949090165619,
3.54957036835372E-17));
#11780=CARTESIAN_POINT('Ctrl Pts',(0.19235503384787,-7.62302506290143,1.08425633614596E-17));
#11781=CARTESIAN_POINT('Ctrl Pts',(0.188962047141393,-7.62647538090844,
6.93889390390723E-18));
#11782=CARTESIAN_POINT('Ctrl Pts',(0.179751979430083,-7.63584107114516,
-3.65739283013793E-18));
#11783=CARTESIAN_POINT('Ctrl Pts',(0.169961756459919,-7.64460258732274,
1.58981699072491E-17));
#11784=CARTESIAN_POINT('Ctrl Pts',(0.15965473466309,-7.65269275268246,1.73472347597681E-17));
#11785=CARTESIAN_POINT('Ctrl Pts',(0.154922700033441,-7.6564070111168,1.80125118104906E-17));
#11786=CARTESIAN_POINT('Ctrl Pts',(0.150081554712747,-7.65997966275367,
2.66878873465253E-17));
#11787=CARTESIAN_POINT('Ctrl Pts',(0.145136600582228,-7.66340356863892,
3.81639164714898E-17));
#11788=CARTESIAN_POINT('Ctrl Pts',(0.139976052344163,-7.66697675274073,
5.01402867911481E-17));
#11789=CARTESIAN_POINT('Ctrl Pts',(0.134708897983985,-7.67038332088609,
-3.16234153219695E-17));
#11790=CARTESIAN_POINT('Ctrl Pts',(0.129346789376753,-7.67361307290272,
-1.73472347597681E-17));
#11791=CARTESIAN_POINT('Ctrl Pts',(0.117404965946791,-7.68080597612983,
1.44469044522131E-17));
#11792=CARTESIAN_POINT('Ctrl Pts',(0.10498570886698,-7.68712791357992,2.06413296011656E-17));
#11793=CARTESIAN_POINT('Ctrl Pts',(0.0921567849037076,-7.69249315206613,
-2.08166817117217E-17));
#11794=CARTESIAN_POINT('Ctrl Pts',(0.0880066762640415,-7.69422878653238,
-3.42281924062706E-17));
#11795=CARTESIAN_POINT('Ctrl Pts',(0.0838136017590666,-7.69586419192416,
-4.59422420206302E-18));
#11796=CARTESIAN_POINT('Ctrl Pts',(0.0795809081573363,-7.69740028961993,
-6.93889390390723E-18));
#11797=CARTESIAN_POINT('Ctrl Pts',(-0.2516645197469,-7.40021351101923,-0.161258330249198));
#11798=CARTESIAN_POINT('Ctrl Pts',(-0.251853760397228,-7.42268031128274,
-0.15983892928355));
#11799=CARTESIAN_POINT('Ctrl Pts',(-0.249087077319634,-7.445101303405,-0.158419528317902));
#11800=CARTESIAN_POINT('Ctrl Pts',(-0.243177161464371,-7.46666062885335,
-0.157000127352254));
#11801=CARTESIAN_POINT('Ctrl Pts',(-0.221387275816053,-7.54614995622776,
-0.151766789773845));
#11802=CARTESIAN_POINT('Ctrl Pts',(-0.156868279689982,-7.61392578571347,
-0.146533452195437));
#11803=CARTESIAN_POINT('Ctrl Pts',(-0.0785474567930319,-7.63960158320207,
-0.141300114617028));
#11804=CARTESIAN_POINT('Ctrl Pts',(-0.000226633896081616,-7.66527738069067,
-0.13606677703862));
#11805=CARTESIAN_POINT('Ctrl Pts',(0.0918960157717476,-7.64885314618216,
-0.130833439460211));
#11806=CARTESIAN_POINT('Ctrl Pts',(0.156516622945739,-7.59769057715216,
-0.125600101881803));
#11807=CARTESIAN_POINT('Ctrl Pts',(0.22113723011973,-7.54652800812215,-0.120366764303394));
#11808=CARTESIAN_POINT('Ctrl Pts',(0.258255794799884,-7.46062710457066,
-0.115133426724986));
#11809=CARTESIAN_POINT('Ctrl Pts',(0.251230509311017,-7.37850635978343,
-0.109900089146578));
#11810=CARTESIAN_POINT('Ctrl Pts',(0.244205223822151,-7.2963856149962,-0.104666751568169));
#11811=CARTESIAN_POINT('Ctrl Pts',(0.193036088164265,-7.21804502897323,
-0.0994334139897607));
#11812=CARTESIAN_POINT('Ctrl Pts',(0.120664063886602,-7.17860008142513,
-0.0942000764113522));
#11813=CARTESIAN_POINT('Ctrl Pts',(0.048292039608938,-7.13915513387703,
-0.0889667388329437));
#11814=CARTESIAN_POINT('Ctrl Pts',(-0.0452828732885026,-7.13860582480379,
-0.0837334012545353));
#11815=CARTESIAN_POINT('Ctrl Pts',(-0.118103965820357,-7.177216388362,-0.0785000636761268));
#11816=CARTESIAN_POINT('Ctrl Pts',(-0.190925058352211,-7.21582695192021,
-0.0732667260977184));
#11817=CARTESIAN_POINT('Ctrl Pts',(-0.242992330518479,-7.29359738810986,
-0.06803338851931));
#11818=CARTESIAN_POINT('Ctrl Pts',(-0.250965095861989,-7.37562273179982,
-0.0628000509409015));
#11819=CARTESIAN_POINT('Ctrl Pts',(-0.251748010978523,-7.3836775131394,
-0.062286144043667));
#11820=CARTESIAN_POINT('Ctrl Pts',(-0.252105723523339,-7.3917733244789,
-0.0617722371464325));
#11821=CARTESIAN_POINT('Ctrl Pts',(-0.25205356191611,-7.39987360404796,
-0.0612583302491979));
#11822=CARTESIAN_POINT('Ctrl Pts',(-0.0793799282532839,-7.69692229537457,
2.77555756156289E-17));
#11823=CARTESIAN_POINT('Ctrl Pts',(-0.177014005842305,-7.67082056372685,
-0.00523333757840842));
#11824=CARTESIAN_POINT('Ctrl Pts',(-0.342929400138797,-7.51523794788106,
-0.0157000127352253));
#11825=CARTESIAN_POINT('Ctrl Pts',(-0.285303631037492,-7.17698397189122,
-0.0314000254704507));
#11826=CARTESIAN_POINT('Ctrl Pts',(0.0286357521188298,-7.03927813304723,
-0.047100038205676));
#11827=CARTESIAN_POINT('Ctrl Pts',(0.31666225793602,-7.22476085896309,-0.0628000509409014));
#11828=CARTESIAN_POINT('Ctrl Pts',(0.320850989126134,-7.56751742991046,
-0.0785000636761266));
#11829=CARTESIAN_POINT('Ctrl Pts',(0.0372719144191142,-7.75999252270946,
-0.0942000764113521));
#11830=CARTESIAN_POINT('Ctrl Pts',(-0.27970066815779,-7.62969207265103,
-0.109900089146577));
#11831=CARTESIAN_POINT('Ctrl Pts',(-0.345877143550449,-7.29340807693237,
-0.125600101881803));
#11832=CARTESIAN_POINT('Ctrl Pts',(-0.101895244140074,-7.05271424100694,
-0.141300114617028));
#11833=CARTESIAN_POINT('Ctrl Pts',(0.233453617301762,-7.1234308319262,-0.157000127352253));
#11834=CARTESIAN_POINT('Ctrl Pts',(0.359464106016436,-7.44215165429935,
-0.172700140087479));
#11835=CARTESIAN_POINT('Ctrl Pts',(0.163138826931865,-7.72307368988404,
-0.188400152822704));
#11836=CARTESIAN_POINT('Ctrl Pts',(-0.179474179312067,-7.714292941062,-0.204100165557929));
#11837=CARTESIAN_POINT('Ctrl Pts',(-0.36115117737076,-7.42368245253896,
-0.219800178293155));
#11838=CARTESIAN_POINT('Ctrl Pts',(-0.218980345752975,-7.11183580270963,
-0.23550019102838));
#11839=CARTESIAN_POINT('Ctrl Pts',(0.119552211049655,-7.05838869308885,
-0.251200203763606));
#11840=CARTESIAN_POINT('Ctrl Pts',(0.350881178877997,-7.31126774940073,
-0.266900216498831));
#11841=CARTESIAN_POINT('Ctrl Pts',(0.267571614711511,-7.64371385133353,
-0.282600229234056));
#11842=CARTESIAN_POINT('Ctrl Pts',(-0.0556719770403169,-7.75761941200269,
-0.298300241969282));
#11843=CARTESIAN_POINT('Ctrl Pts',(-0.328993976006532,-7.55084421145899,
-0.314000254704507));
#11844=CARTESIAN_POINT('Ctrl Pts',(-0.307303918916174,-7.20880556116322,
-0.329700267439732));
#11845=CARTESIAN_POINT('Ctrl Pts',(-0.0100514903598289,-7.03821279751757,
-0.345400280174958));
#11846=CARTESIAN_POINT('Ctrl Pts',(0.296214206411665,-7.19203808960976,
-0.361100292910183));
#11847=CARTESIAN_POINT('Ctrl Pts',(0.336861782355269,-7.53234482162411,
-0.376800305645408));
#11848=CARTESIAN_POINT('Ctrl Pts',(0.0754421664482044,-7.75397668254217,
-0.392500318380634));
#11849=CARTESIAN_POINT('Ctrl Pts',(-0.253627163917688,-7.65819425626374,
-0.408200331115859));
#11850=CARTESIAN_POINT('Ctrl Pts',(-0.355266583188697,-7.3308865634341,
-0.423900343851084));
#11851=CARTESIAN_POINT('Ctrl Pts',(-0.138335049048699,-7.06555355216919,
-0.43960035658631));
#11852=CARTESIAN_POINT('Ctrl Pts',(0.202642850697595,-7.1001218792852,-0.455300369321535));
#11853=CARTESIAN_POINT('Ctrl Pts',(0.361908962168568,-7.40359379400104,
-0.47100038205676));
#11854=CARTESIAN_POINT('Ctrl Pts',(0.196647835235759,-7.70384311944753,
-0.486700394791986));
#11855=CARTESIAN_POINT('Ctrl Pts',(-0.144949292044521,-7.73163340416662,
-0.502400407527211));
#11856=CARTESIAN_POINT('Ctrl Pts',(-0.356568998694743,-7.46204483499129,
-0.518100420262437));
#11857=CARTESIAN_POINT('Ctrl Pts',(-0.24844986319099,-7.13682006469127,
-0.533800432997662));
#11858=CARTESIAN_POINT('Ctrl Pts',(0.0824566476388583,-7.04759127197059,
-0.549500445732887));
#11859=CARTESIAN_POINT('Ctrl Pts',(0.3394234925214,-7.27437075694011,-0.565200458468112));
#11860=CARTESIAN_POINT('Ctrl Pts',(0.292026033272937,-7.61380320873943,
-0.580900471203338));
#11861=CARTESIAN_POINT('Ctrl Pts',(-0.0172339673348224,-7.76151623310164,
-0.596600483938563));
#11862=CARTESIAN_POINT('Ctrl Pts',(-0.311040112666544,-7.58505426173674,
-0.612300496673788));
#11863=CARTESIAN_POINT('Ctrl Pts',(-0.325933587701845,-7.24265219973275,
-0.628000509409014));
#11864=CARTESIAN_POINT('Ctrl Pts',(-0.0485593226474429,-7.04134574011728,
-0.643700522144239));
#11865=CARTESIAN_POINT('Ctrl Pts',(0.272358623219876,-7.16164734985291,
-0.659400534879465));
#11866=CARTESIAN_POINT('Ctrl Pts',(0.349049836864763,-7.49568337130869,
-0.675100547614689));
#11867=CARTESIAN_POINT('Ctrl Pts',(0.11274499939327,-7.74391656588417,-0.690800560349915));
#11868=CARTESIAN_POINT('Ctrl Pts',(-0.224659938070643,-7.68376178164081,
-0.706500573085141));
#11869=CARTESIAN_POINT('Ctrl Pts',(-0.360608988983327,-7.36914438347625,
-0.722200585820365));
#11870=CARTESIAN_POINT('Ctrl Pts',(-0.173198849645488,-7.08221710163593,
-0.737900598555592));
#11871=CARTESIAN_POINT('Ctrl Pts',(0.169525099592154,-7.08020524213913,
-0.753600611290816));
#11872=CARTESIAN_POINT('Ctrl Pts',(0.360224706479889,-7.36504427094214,
-0.769300624026043));
#11873=CARTESIAN_POINT('Ctrl Pts',(0.227926616839064,-7.68105111445003,
-0.785000636761266));
#11874=CARTESIAN_POINT('Ctrl Pts',(-0.108793742993405,-7.74539576164464,
-0.800700649496493));
#11875=CARTESIAN_POINT('Ctrl Pts',(-0.347884343277012,-7.49928162878455,
-0.816400662231718));
#11876=CARTESIAN_POINT('Ctrl Pts',(-0.299281595044583,-7.27708432618564,
-0.826867337388535));
#11877=CARTESIAN_POINT('Ctrl Pts',(-0.233606265769615,-7.20026984430694,
-0.832100674966943));
#11878=CARTESIAN_POINT('Ctrl Pts',(-0.074593285434692,-7.67901775698422,
0.0107002249889811));
#11879=CARTESIAN_POINT('Ctrl Pts',(-0.166339987378195,-7.65448997065358,
0.00546688741057264));
#11880=CARTESIAN_POINT('Ctrl Pts',(-0.322250614120992,-7.50828905150648,
-0.00499978774624427));
#11881=CARTESIAN_POINT('Ctrl Pts',(-0.268099702958013,-7.19043193150604,
-0.0206998004814696));
#11882=CARTESIAN_POINT('Ctrl Pts',(0.0269090043092675,-7.06102981224313,
-0.036399813216695));
#11883=CARTESIAN_POINT('Ctrl Pts',(0.297567391560831,-7.23532785233835,
-0.0520998259519202));
#11884=CARTESIAN_POINT('Ctrl Pts',(0.301503540511186,-7.55741605894031,
-0.0677998386871457));
#11885=CARTESIAN_POINT('Ctrl Pts',(0.0350244024168338,-7.73828482327598,
-0.0834998514223709));
#11886=CARTESIAN_POINT('Ctrl Pts',(-0.262834601079461,-7.61584154476274,
-0.0991998641575964));
#11887=CARTESIAN_POINT('Ctrl Pts',(-0.325020607374097,-7.29983561440058,
-0.114899876892822));
#11888=CARTESIAN_POINT('Ctrl Pts',(-0.0957509183722879,-7.07365571728264,
-0.130599889628047));
#11889=CARTESIAN_POINT('Ctrl Pts',(0.219376266700408,-7.14010806824191,
-0.146299902363272));
#11890=CARTESIAN_POINT('Ctrl Pts',(0.337788270330178,-7.43960989194476,
-0.161999915098498));
#11891=CARTESIAN_POINT('Ctrl Pts',(0.153301487549606,-7.70359221148531,
-0.177699927833723));
#11892=CARTESIAN_POINT('Ctrl Pts',(-0.168651811360491,-7.69534094548361,
-0.193399940568948));
#11893=CARTESIAN_POINT('Ctrl Pts',(-0.339373610577404,-7.42225439076231,
-0.209099953304174));
#11894=CARTESIAN_POINT('Ctrl Pts',(-0.205775739469297,-7.12921222412858,
-0.224799966039399));
#11895=CARTESIAN_POINT('Ctrl Pts',(0.112343162804592,-7.07898799753467,
-0.240499978774624));
#11896=CARTESIAN_POINT('Ctrl Pts',(0.329722897281971,-7.31661834116182,
-0.25619999150985));
#11897=CARTESIAN_POINT('Ctrl Pts',(0.251436934620453,-7.62901780433593,
-0.271900004245075));
#11898=CARTESIAN_POINT('Ctrl Pts',(-0.0523149335790711,-7.73605481213571,
-0.287600016980301));
#11899=CARTESIAN_POINT('Ctrl Pts',(-0.309155501882608,-7.54174824252333,
-0.303300029715526));
#11900=CARTESIAN_POINT('Ctrl Pts',(-0.288773364291437,-7.22033466565791,
-0.319000042450751));
#11901=CARTESIAN_POINT('Ctrl Pts',(-0.00944538129415302,-7.06002871689073,
-0.334700055185977));
#11902=CARTESIAN_POINT('Ctrl Pts',(0.278352366081435,-7.20457827964033,
-0.350400067921202));
#11903=CARTESIAN_POINT('Ctrl Pts',(0.316548876223331,-7.52436437361988,
-0.366100080656427));
#11904=CARTESIAN_POINT('Ctrl Pts',(0.0708929723106632,-7.73263174078266,
-0.381800093391653));
#11905=CARTESIAN_POINT('Ctrl Pts',(-0.238333340031973,-7.64262503480259,
-0.397500106126878));
#11906=CARTESIAN_POINT('Ctrl Pts',(-0.333843859881619,-7.33505413251718,
-0.413200118862103));
#11907=CARTESIAN_POINT('Ctrl Pts',(-0.12999338782956,-7.08572081262079,
-0.428900131597328));
#11908=CARTESIAN_POINT('Ctrl Pts',(0.190423402187442,-7.11820465517776,
-0.444600144332554));
#11909=CARTESIAN_POINT('Ctrl Pts',(0.340085700635493,-7.4033770867222,-0.460300157067779));
#11910=CARTESIAN_POINT('Ctrl Pts',(0.184789888661161,-7.6855212524758,-0.476000169803005));
#11911=CARTESIAN_POINT('Ctrl Pts',(-0.13620878921097,-7.71163577142256,
-0.491700182538229));
#11912=CARTESIAN_POINT('Ctrl Pts',(-0.33506773918883,-7.45830350553463,
-0.507400195273456));
#11913=CARTESIAN_POINT('Ctrl Pts',(-0.233468232700866,-7.15268992468061,
-0.52310020800868));
#11914=CARTESIAN_POINT('Ctrl Pts',(0.0774844773566386,-7.06884166541827,
-0.538800220743906));
#11915=CARTESIAN_POINT('Ctrl Pts',(0.318956114196808,-7.28194625275284,
-0.554500233479131));
#11916=CARTESIAN_POINT('Ctrl Pts',(0.274416741531735,-7.60091078597937,
-0.570200246214357));
#11917=CARTESIAN_POINT('Ctrl Pts',(-0.0161947519085262,-7.73971665329528,
-0.585900258949582));
#11918=CARTESIAN_POINT('Ctrl Pts',(-0.292284263998619,-7.57389541248501,
-0.601600271684807));
#11919=CARTESIAN_POINT('Ctrl Pts',(-0.306279656270553,-7.2521403377891,
-0.617300284420032));
#11920=CARTESIAN_POINT('Ctrl Pts',(-0.0456311752159611,-7.06297274174353,
-0.633000297155258));
#11921=CARTESIAN_POINT('Ctrl Pts',(0.255935284516958,-7.17602011418042,
-0.648700309890483));
#11922=CARTESIAN_POINT('Ctrl Pts',(0.328001985956807,-7.48991362406639,
-0.664400322625709));
#11923=CARTESIAN_POINT('Ctrl Pts',(0.105946428853423,-7.72317825335973,
-0.680100335360934));
#11924=CARTESIAN_POINT('Ctrl Pts',(-0.211112849998708,-7.66665082772375,
-0.695800348096159));
#11925=CARTESIAN_POINT('Ctrl Pts',(-0.338864116376122,-7.37100499003633,
-0.711500360831385));
#11926=CARTESIAN_POINT('Ctrl Pts',(-0.162754886693057,-7.10137954309684,
-0.72720037356661));
#11927=CARTESIAN_POINT('Ctrl Pts',(0.159302665301906,-7.09948899956776,
-0.742900386301835));
#11928=CARTESIAN_POINT('Ctrl Pts',(0.338503006268098,-7.36715211600001,
-0.758600399037061));
#11929=CARTESIAN_POINT('Ctrl Pts',(0.214182546673399,-7.66410361489641,
-0.774300411772286));
#11930=CARTESIAN_POINT('Ctrl Pts',(-0.102233434864309,-7.7245682529982,
-0.790000424507512));
#11931=CARTESIAN_POINT('Ctrl Pts',(-0.326906772119047,-7.49329490511401,
-0.805700437242737));
#11932=CARTESIAN_POINT('Ctrl Pts',(-0.281234789899006,-7.28449619263982,
-0.816167112399554));
#11933=CARTESIAN_POINT('Ctrl Pts',(-0.219519710401912,-7.21231365609213,
-0.821400449977962));
#11934=CARTESIAN_POINT('Ctrl Pts',(-0.0698066426161,-7.66111321859386,0.0214004499779622));
#11935=CARTESIAN_POINT('Ctrl Pts',(-0.155665968914086,-7.6381593775803,
0.0161671123995537));
#11936=CARTESIAN_POINT('Ctrl Pts',(-0.301571828103187,-7.50134015513189,
0.00570043724273681));
#11937=CARTESIAN_POINT('Ctrl Pts',(-0.250895774878533,-7.20387989112088,
-0.00999957549248853));
#11938=CARTESIAN_POINT('Ctrl Pts',(0.0251822564997051,-7.08278149143901,
-0.0256995882277139));
#11939=CARTESIAN_POINT('Ctrl Pts',(0.278472525185642,-7.2458948457136,-0.0413996009629392));
#11940=CARTESIAN_POINT('Ctrl Pts',(0.282156091896237,-7.54731468797016,
-0.0570996136981646));
#11941=CARTESIAN_POINT('Ctrl Pts',(0.0327768904145534,-7.7165771238425,
-0.0727996264333898));
#11942=CARTESIAN_POINT('Ctrl Pts',(-0.245968534001132,-7.60199101687444,
-0.0884996391686154));
#11943=CARTESIAN_POINT('Ctrl Pts',(-0.304164071197746,-7.30626315186879,
-0.10419965190384));
#11944=CARTESIAN_POINT('Ctrl Pts',(-0.0896065926045006,-7.09459719355835,
-0.119899664639066));
#11945=CARTESIAN_POINT('Ctrl Pts',(0.205298916099055,-7.15678530455762,
-0.135599677374291));
#11946=CARTESIAN_POINT('Ctrl Pts',(0.316112434643921,-7.43706812959018,
-0.151299690109517));
#11947=CARTESIAN_POINT('Ctrl Pts',(0.143464148167348,-7.68411073308658,
-0.166999702844742));
#11948=CARTESIAN_POINT('Ctrl Pts',(-0.157829443408914,-7.67638894990523,
-0.182699715579967));
#11949=CARTESIAN_POINT('Ctrl Pts',(-0.317596043784047,-7.42082632898565,
-0.198399728315193));
#11950=CARTESIAN_POINT('Ctrl Pts',(-0.192571133185619,-7.14658864554754,
-0.214099741050418));
#11951=CARTESIAN_POINT('Ctrl Pts',(0.105134114559528,-7.09958730198047,
-0.229799753785643));
#11952=CARTESIAN_POINT('Ctrl Pts',(0.308564615685943,-7.32196893292292,
-0.245499766520869));
#11953=CARTESIAN_POINT('Ctrl Pts',(0.235302254529395,-7.61432175733832,
-0.261199779256094));
#11954=CARTESIAN_POINT('Ctrl Pts',(-0.0489578901178251,-7.71449021226873,
-0.276899791991319));
#11955=CARTESIAN_POINT('Ctrl Pts',(-0.289317027758686,-7.53265227358768,
-0.292599804726545));
#11956=CARTESIAN_POINT('Ctrl Pts',(-0.270242809666699,-7.2318637701526,
-0.30829981746177));
#11957=CARTESIAN_POINT('Ctrl Pts',(-0.00883927222847752,-7.08184463626389,
-0.323999830196995));
#11958=CARTESIAN_POINT('Ctrl Pts',(0.260490525751205,-7.21711846967092,
-0.339699842932221));
#11959=CARTESIAN_POINT('Ctrl Pts',(0.296235970091394,-7.51638392561565,
-0.355399855667446));
#11960=CARTESIAN_POINT('Ctrl Pts',(0.0663437781731218,-7.71128679902317,
-0.371099868402672));
#11961=CARTESIAN_POINT('Ctrl Pts',(-0.223039516146258,-7.62705581334143,
-0.386799881137897));
#11962=CARTESIAN_POINT('Ctrl Pts',(-0.312421136574541,-7.33922170160028,
-0.402499893873123));
#11963=CARTESIAN_POINT('Ctrl Pts',(-0.12165172661042,-7.10588807307238,
-0.418199906608347));
#11964=CARTESIAN_POINT('Ctrl Pts',(0.17820395367729,-7.13628743107034,-0.433899919343573));
#11965=CARTESIAN_POINT('Ctrl Pts',(0.318262439102417,-7.40316037944335,
-0.449599932078798));
#11966=CARTESIAN_POINT('Ctrl Pts',(0.172931942086563,-7.66719938550407,
-0.465299944814024));
#11967=CARTESIAN_POINT('Ctrl Pts',(-0.127468286377419,-7.69163813867849,
-0.480999957549249));
#11968=CARTESIAN_POINT('Ctrl Pts',(-0.313566479682916,-7.45456217607797,
-0.496699970284474));
#11969=CARTESIAN_POINT('Ctrl Pts',(-0.218486602210741,-7.16855978466994,
-0.512399983019699));
#11970=CARTESIAN_POINT('Ctrl Pts',(0.0725123070744189,-7.09009205886595,
-0.528099995754925));
#11971=CARTESIAN_POINT('Ctrl Pts',(0.298488735872217,-7.28952174856557,
-0.54380000849015));
#11972=CARTESIAN_POINT('Ctrl Pts',(0.256807449790533,-7.58801836321932,
-0.559500021225376));
#11973=CARTESIAN_POINT('Ctrl Pts',(-0.0151555364822303,-7.71791707348892,
-0.5752000339606));
#11974=CARTESIAN_POINT('Ctrl Pts',(-0.273528415330694,-7.56273656323327,
-0.590900046695827));
#11975=CARTESIAN_POINT('Ctrl Pts',(-0.286625724839261,-7.26162847584545,
-0.606600059431051));
#11976=CARTESIAN_POINT('Ctrl Pts',(-0.0427030277844796,-7.08459974336978,
-0.622300072166277));
#11977=CARTESIAN_POINT('Ctrl Pts',(0.239511945814041,-7.19039287850791,
-0.638000084901502));
#11978=CARTESIAN_POINT('Ctrl Pts',(0.306954135048851,-7.4841438768241,-0.653700097636728));
#11979=CARTESIAN_POINT('Ctrl Pts',(0.0991478583135767,-7.70243994083529,
-0.669400110371953));
#11980=CARTESIAN_POINT('Ctrl Pts',(-0.197565761926773,-7.64953987380668,
-0.685100123107178));
#11981=CARTESIAN_POINT('Ctrl Pts',(-0.317119243768918,-7.37286559659641,
-0.700800135842404));
#11982=CARTESIAN_POINT('Ctrl Pts',(-0.152310923740626,-7.12054198455776,
-0.716500148577628));
#11983=CARTESIAN_POINT('Ctrl Pts',(0.149080231011657,-7.11877275699639,
-0.732200161312855));
#11984=CARTESIAN_POINT('Ctrl Pts',(0.316781306056307,-7.36925996105789,
-0.747900174048079));
#11985=CARTESIAN_POINT('Ctrl Pts',(0.200438476507733,-7.64715611534278,
-0.763600186783305));
#11986=CARTESIAN_POINT('Ctrl Pts',(-0.0956731267352124,-7.70374074435177,
-0.779300199518531));
#11987=CARTESIAN_POINT('Ctrl Pts',(-0.305929200961081,-7.48730818144347,
-0.795000212253756));
#11988=CARTESIAN_POINT('Ctrl Pts',(-0.26318798475343,-7.291908059094,-0.805466887410573));
#11989=CARTESIAN_POINT('Ctrl Pts',(-0.205433155034209,-7.22435746787732,
-0.810700224988981));
#11990=CARTESIAN_POINT('Ctrl Pts',(-0.0650199997975081,-7.64320868020351,
0.0321006749669432));
#11991=CARTESIAN_POINT('Ctrl Pts',(-0.144991950449976,-7.62182878450703,
0.0268673373885348));
#11992=CARTESIAN_POINT('Ctrl Pts',(-0.280893042085382,-7.4943912587573,
0.0164006622317179));
#11993=CARTESIAN_POINT('Ctrl Pts',(-0.233691846799053,-7.2173278507357,
0.000700649496492526));
#11994=CARTESIAN_POINT('Ctrl Pts',(0.0234555086901425,-7.10453317063491,
-0.0149993632387329));
#11995=CARTESIAN_POINT('Ctrl Pts',(0.259377658810454,-7.25646183908885,
-0.0306993759739581));
#11996=CARTESIAN_POINT('Ctrl Pts',(0.262808643281289,-7.53721331700002,
-0.0463993887091836));
#11997=CARTESIAN_POINT('Ctrl Pts',(0.030529378412273,-7.694869424409,-0.0620994014444088));
#11998=CARTESIAN_POINT('Ctrl Pts',(-0.229102466922803,-7.58814048898617,
-0.0777994141796343));
#11999=CARTESIAN_POINT('Ctrl Pts',(-0.283307535021394,-7.31269068933698,
-0.0934994269148594));
#12000=CARTESIAN_POINT('Ctrl Pts',(-0.0834622668367136,-7.11553866983406,
-0.109199439650085));
#12001=CARTESIAN_POINT('Ctrl Pts',(0.191221565497701,-7.17346254087333,
-0.12489945238531));
#12002=CARTESIAN_POINT('Ctrl Pts',(0.294436598957663,-7.4345263672356,-0.140599465120536));
#12003=CARTESIAN_POINT('Ctrl Pts',(0.133626808785089,-7.66462925468784,
-0.156299477855761));
#12004=CARTESIAN_POINT('Ctrl Pts',(-0.147007075457338,-7.65743695432686,
-0.171999490590986));
#12005=CARTESIAN_POINT('Ctrl Pts',(-0.295818476990691,-7.41939826720899,
-0.187699503326212));
#12006=CARTESIAN_POINT('Ctrl Pts',(-0.179366526901941,-7.16396506696649,
-0.203399516061437));
#12007=CARTESIAN_POINT('Ctrl Pts',(0.0979250663144644,-7.12018660642628,
-0.219099528796662));
#12008=CARTESIAN_POINT('Ctrl Pts',(0.287406334089916,-7.32731952468401,
-0.234799541531888));
#12009=CARTESIAN_POINT('Ctrl Pts',(0.219167574438337,-7.59962571034071,
-0.250499554267113));
#12010=CARTESIAN_POINT('Ctrl Pts',(-0.0456008466565794,-7.69292561240175,
-0.266199567002338));
#12011=CARTESIAN_POINT('Ctrl Pts',(-0.269478553634763,-7.52355630465202,
-0.281899579737564));
#12012=CARTESIAN_POINT('Ctrl Pts',(-0.251712255041962,-7.24339287464728,
-0.297599592472789));
#12013=CARTESIAN_POINT('Ctrl Pts',(-0.00823316316280154,-7.10366055563705,
-0.313299605208015));
#12014=CARTESIAN_POINT('Ctrl Pts',(0.242628685420975,-7.2296586597015,-0.32899961794324));
#12015=CARTESIAN_POINT('Ctrl Pts',(0.275923063959457,-7.50840347761142,
-0.344699630678465));
#12016=CARTESIAN_POINT('Ctrl Pts',(0.0617945840355804,-7.68994185726368,
-0.36039964341369));
#12017=CARTESIAN_POINT('Ctrl Pts',(-0.207745692260543,-7.61148659188026,
-0.376099656148916));
#12018=CARTESIAN_POINT('Ctrl Pts',(-0.290998413267463,-7.34338927068337,
-0.391799668884141));
#12019=CARTESIAN_POINT('Ctrl Pts',(-0.113310065391281,-7.12605533352397,
-0.407499681619367));
#12020=CARTESIAN_POINT('Ctrl Pts',(0.165984505167137,-7.1543702069629,-0.423199694354592));
#12021=CARTESIAN_POINT('Ctrl Pts',(0.296439177569342,-7.40294367216451,
-0.438899707089817));
#12022=CARTESIAN_POINT('Ctrl Pts',(0.161073995511965,-7.64887751853234,
-0.454599719825043));
#12023=CARTESIAN_POINT('Ctrl Pts',(-0.118727783543868,-7.67164050593443,
-0.470299732560267));
#12024=CARTESIAN_POINT('Ctrl Pts',(-0.292065220177002,-7.4508208466213,
-0.485999745295493));
#12025=CARTESIAN_POINT('Ctrl Pts',(-0.203504971720617,-7.18442964465928,
-0.501699758030718));
#12026=CARTESIAN_POINT('Ctrl Pts',(0.0675401367921992,-7.11134245231363,
-0.517399770765944));
#12027=CARTESIAN_POINT('Ctrl Pts',(0.278021357547625,-7.29709724437831,
-0.533099783501169));
#12028=CARTESIAN_POINT('Ctrl Pts',(0.239198158049331,-7.57512594045925,
-0.548799796236395));
#12029=CARTESIAN_POINT('Ctrl Pts',(-0.0141163210559342,-7.69611749368257,
-0.56449980897162));
#12030=CARTESIAN_POINT('Ctrl Pts',(-0.25477256666277,-7.55157771398154,
-0.580199821706845));
#12031=CARTESIAN_POINT('Ctrl Pts',(-0.26697179340797,-7.2711166139018,-0.595899834442071));
#12032=CARTESIAN_POINT('Ctrl Pts',(-0.0397748803529979,-7.10622674499603,
-0.611599847177296));
#12033=CARTESIAN_POINT('Ctrl Pts',(0.223088607111123,-7.20476564283543,
-0.627299859912521));
#12034=CARTESIAN_POINT('Ctrl Pts',(0.285906284140895,-7.47837412958179,
-0.642999872647747));
#12035=CARTESIAN_POINT('Ctrl Pts',(0.0923492877737298,-7.68170162831085,
-0.658699885382972));
#12036=CARTESIAN_POINT('Ctrl Pts',(-0.184018673854838,-7.63242891988962,
-0.674399898118197));
#12037=CARTESIAN_POINT('Ctrl Pts',(-0.295374371161713,-7.37472620315649,
-0.690099910853423));
#12038=CARTESIAN_POINT('Ctrl Pts',(-0.141866960788195,-7.13970442601869,
-0.705799923588648));
#12039=CARTESIAN_POINT('Ctrl Pts',(0.138857796721408,-7.13805651442501,
-0.721499936323874));
#12040=CARTESIAN_POINT('Ctrl Pts',(0.295059605844517,-7.37136780611577,
-0.737199949059099));
#12041=CARTESIAN_POINT('Ctrl Pts',(0.186694406342068,-7.63020861578915,
-0.752899961794324));
#12042=CARTESIAN_POINT('Ctrl Pts',(-0.0891128186061158,-7.68291323570534,
-0.76859997452955));
#12043=CARTESIAN_POINT('Ctrl Pts',(-0.284951629803116,-7.48132145777293,
-0.784299987264774));
#12044=CARTESIAN_POINT('Ctrl Pts',(-0.245141179607853,-7.29931992554818,
-0.794766662421592));
#12045=CARTESIAN_POINT('Ctrl Pts',(-0.191346599666506,-7.23640127966251,
-0.8));
#12046=CARTESIAN_POINT('Ctrl Pts',(-0.191346599666506,-7.23640127966251,
-0.8));
#12047=CARTESIAN_POINT('Ctrl Pts',(-0.202509812150815,-7.24689195824451,
-0.8));
#12048=CARTESIAN_POINT('Ctrl Pts',(-0.21257001858597,-7.25841324529628,
-0.8));
#12049=CARTESIAN_POINT('Ctrl Pts',(-0.2215222854557,-7.27074763835105,-0.8));
#12050=CARTESIAN_POINT('Ctrl Pts',(-0.229528851949894,-7.28177904967911,
-0.8));
#12051=CARTESIAN_POINT('Ctrl Pts',(-0.236649218441325,-7.29346217849914,
-0.8));
#12052=CARTESIAN_POINT('Ctrl Pts',(-0.242860433713407,-7.30566893142592,
-0.8));
#12053=CARTESIAN_POINT('Ctrl Pts',(-0.244940810611317,-7.30975744642258,
-0.8));
#12054=CARTESIAN_POINT('Ctrl Pts',(-0.246919675168011,-7.31390635200313,
-0.8));
#12055=CARTESIAN_POINT('Ctrl Pts',(-0.248793541339973,-7.31810664328013,
-0.8));
#12056=CARTESIAN_POINT('Ctrl Pts',(-0.255493751071069,-7.33312523580754,
-0.8));
#12057=CARTESIAN_POINT('Ctrl Pts',(-0.260811073903805,-7.34869792479653,
-0.8));
#12058=CARTESIAN_POINT('Ctrl Pts',(-0.264722800485284,-7.36459862853377,
-0.8));
#12059=CARTESIAN_POINT('Ctrl Pts',(-0.267427531006873,-7.37559303671058,
-0.8));
#12060=CARTESIAN_POINT('Ctrl Pts',(-0.269459584929932,-7.38674533385887,
-0.8));
#12061=CARTESIAN_POINT('Ctrl Pts',(-0.270799630246209,-7.39798910408356,
-0.8));
#12062=CARTESIAN_POINT('Ctrl Pts',(-0.271554584183732,-7.40432361270102,
-0.8));
#12063=CARTESIAN_POINT('Ctrl Pts',(-0.272089709263086,-7.41068724824774,
-0.8));
#12064=CARTESIAN_POINT('Ctrl Pts',(-0.272399954519056,-7.41706856176779,
-0.8));
#12065=CARTESIAN_POINT('Ctrl Pts',(-0.272610215830843,-7.42139334458343,
-0.8));
#12066=CARTESIAN_POINT('Ctrl Pts',(-0.272716688467774,-7.42571717942635,
-0.8));
#12067=CARTESIAN_POINT('Ctrl Pts',(-0.272718878845034,-7.43003460508684,
-0.8));
#12068=CARTESIAN_POINT('Ctrl Pts',(-0.272726877365373,-7.44580039008993,
-0.8));
#12069=CARTESIAN_POINT('Ctrl Pts',(-0.271347528745165,-7.46148685548989,
-0.8));
#12070=CARTESIAN_POINT('Ctrl Pts',(-0.268538072982214,-7.47691819603078,
-0.8));
#12071=CARTESIAN_POINT('Ctrl Pts',(-0.266219589118033,-7.48965280268256,
-0.8));
#12072=CARTESIAN_POINT('Ctrl Pts',(-0.26292668789853,-7.5022143616876,-0.8));
#12073=CARTESIAN_POINT('Ctrl Pts',(-0.258732571736959,-7.51453557833684,
-0.8));
#12074=CARTESIAN_POINT('Ctrl Pts',(-0.256787738588096,-7.52024898961365,
-0.8));
#12075=CARTESIAN_POINT('Ctrl Pts',(-0.254646822394779,-7.52591466429966,
-0.8));
#12076=CARTESIAN_POINT('Ctrl Pts',(-0.252327841578967,-7.53149910592954,
-0.8));
#12077=CARTESIAN_POINT('Ctrl Pts',(-0.245813410497626,-7.54718679936692,
-0.8));
#12078=CARTESIAN_POINT('Ctrl Pts',(-0.237886859352545,-7.56227243122225,
-0.8));
#12079=CARTESIAN_POINT('Ctrl Pts',(-0.228725832616534,-7.57661351587103,
-0.8));
#12080=CARTESIAN_POINT('Ctrl Pts',(-0.223374474548107,-7.58499077327424,
-0.8));
#12081=CARTESIAN_POINT('Ctrl Pts',(-0.217600846214963,-7.59311397793835,
-0.8));
#12082=CARTESIAN_POINT('Ctrl Pts',(-0.21143274247831,-7.60095296973045,
-0.8));
#12083=CARTESIAN_POINT('Ctrl Pts',(-0.20742008137373,-7.60605262738963,
-0.8));
#12084=CARTESIAN_POINT('Ctrl Pts',(-0.203240363216825,-7.61103196707157,
-0.8));
#12085=CARTESIAN_POINT('Ctrl Pts',(-0.19890016925924,-7.6158820614063,-0.8));
#12086=CARTESIAN_POINT('Ctrl Pts',(-0.195670588103427,-7.61949106446479,
-0.8));
#12087=CARTESIAN_POINT('Ctrl Pts',(-0.192354860452395,-7.62302525643464,
-0.8));
#12088=CARTESIAN_POINT('Ctrl Pts',(-0.188961839362612,-7.62647560355552,
-0.8));
#12089=CARTESIAN_POINT('Ctrl Pts',(-0.179751748624594,-7.63584130132751,
-0.8));
#12090=CARTESIAN_POINT('Ctrl Pts',(-0.169961500633801,-7.64460282207988,
-0.8));
#12091=CARTESIAN_POINT('Ctrl Pts',(-0.159654451890089,-7.65269298880017,
-0.8));
#12092=CARTESIAN_POINT('Ctrl Pts',(-0.154923544879998,-7.656406353062,-0.8));
#12093=CARTESIAN_POINT('Ctrl Pts',(-0.150083579318515,-7.65997817804833,
-0.8));
#12094=CARTESIAN_POINT('Ctrl Pts',(-0.145139853312966,-7.66340132998996,
-0.8));
#12095=CARTESIAN_POINT('Ctrl Pts',(-0.13997839750837,-7.66697524315572,
-0.8));
#12096=CARTESIAN_POINT('Ctrl Pts',(-0.134710287969361,-7.67038248469088,
-0.8));
#12097=CARTESIAN_POINT('Ctrl Pts',(-0.129347191444159,-7.67361284285922,
-0.8));
#12098=CARTESIAN_POINT('Ctrl Pts',(-0.117405249048123,-7.68080584246004,
-0.8));
#12099=CARTESIAN_POINT('Ctrl Pts',(-0.104985860997357,-7.68712785830345,
-0.8));
#12100=CARTESIAN_POINT('Ctrl Pts',(-0.0921567961212457,-7.69249315468034,
-0.8));
#12101=CARTESIAN_POINT('Ctrl Pts',(-0.0880066881472035,-7.69422878853143,
-0.8));
#12102=CARTESIAN_POINT('Ctrl Pts',(-0.0838136142204832,-7.69586419339144,
-0.8));
#12103=CARTESIAN_POINT('Ctrl Pts',(-0.0795809211152283,-7.69740029063291,
-0.8));
#12104=CARTESIAN_POINT('Ctrl Pts',(-0.251593604700942,-7.39979879766985,
-0.0887416697508022));
#12105=CARTESIAN_POINT('Ctrl Pts',(-0.251789073617808,-7.37467806093596,
-0.090327588805488));
#12106=CARTESIAN_POINT('Ctrl Pts',(-0.248321652469561,-7.3496099888614,
-0.0919135078601738));
#12107=CARTESIAN_POINT('Ctrl Pts',(-0.240965812307516,-7.32574031936136,
-0.0934994269148596));
#12108=CARTESIAN_POINT('Ctrl Pts',(-0.216692445626501,-7.24697334950268,
-0.0987327644932681));
#12109=CARTESIAN_POINT('Ctrl Pts',(-0.150077356231607,-7.18125600966837,
-0.103966102071677));
#12110=CARTESIAN_POINT('Ctrl Pts',(-0.0709891728117581,-7.15805131825776,
-0.109199439650085));
#12111=CARTESIAN_POINT('Ctrl Pts',(0.00809901060809128,-7.13484662684715,
-0.114432777228494));
#12112=CARTESIAN_POINT('Ctrl Pts',(0.0996602880528962,-7.15415458386024,
-0.119666114806902));
#12113=CARTESIAN_POINT('Ctrl Pts',(0.162643432351959,-7.20731920009383,
-0.12489945238531));
#12114=CARTESIAN_POINT('Ctrl Pts',(0.225626576651022,-7.26048381632742,
-0.130132789963719));
#12115=CARTESIAN_POINT('Ctrl Pts',(0.260031587804342,-7.34750509178151,
-0.135366127542127));
#12116=CARTESIAN_POINT('Ctrl Pts',(0.250432461685574,-7.4293662107506,-0.140599465120536));
#12117=CARTESIAN_POINT('Ctrl Pts',(0.240833335566805,-7.51122732971968,
-0.145832802698944));
#12118=CARTESIAN_POINT('Ctrl Pts',(0.187230072175947,-7.58792829220376,
-0.151066140277353));
#12119=CARTESIAN_POINT('Ctrl Pts',(0.113656126440114,-7.62508005671897,
-0.156299477855761));
#12120=CARTESIAN_POINT('Ctrl Pts',(0.0400821807042802,-7.66223182123418,
-0.161532815434169));
#12121=CARTESIAN_POINT('Ctrl Pts',(-0.0534624473765288,-7.65983438778052,
-0.166766153012578));
#12122=CARTESIAN_POINT('Ctrl Pts',(-0.125036661672492,-7.61896255653404,
-0.171999490590986));
#12123=CARTESIAN_POINT('Ctrl Pts',(-0.196610875968456,-7.57809072528757,
-0.177232828169395));
#12124=CARTESIAN_POINT('Ctrl Pts',(-0.246214676479574,-7.49874449624828,
-0.182466165747803));
#12125=CARTESIAN_POINT('Ctrl Pts',(-0.251607918387007,-7.41649918168822,
-0.187699503326212));
#12126=CARTESIAN_POINT('Ctrl Pts',(-0.251965921640279,-7.41103973991196,
-0.188046892134409));
#12127=CARTESIAN_POINT('Ctrl Pts',(-0.252129119871954,-7.40556752389274,
-0.188394280942605));
#12128=CARTESIAN_POINT('Ctrl Pts',(-0.252102603566075,-7.4000936994049,
-0.188741669750802));
#12129=CARTESIAN_POINT('Ctrl Pts',(-0.0793799282532839,-7.69692229537457,
2.77555756156289E-17));
#12130=CARTESIAN_POINT('Ctrl Pts',(-0.0961911494322625,-7.69077267557206,
2.35324001622483E-17));
#12131=CARTESIAN_POINT('Ctrl Pts',(-0.112330835541762,-7.68307124215404,
-2.1766246802835E-17));
#12132=CARTESIAN_POINT('Ctrl Pts',(-0.127669379580378,-7.67400023063824,
-1.34441069388203E-17));
#12133=CARTESIAN_POINT('Ctrl Pts',(-0.13764508202298,-7.66810073251721,
-8.03165118290813E-18));
#12134=CARTESIAN_POINT('Ctrl Pts',(-0.147281472230525,-7.66162083730929,
2.61489825013166E-18));
#12135=CARTESIAN_POINT('Ctrl Pts',(-0.156535274241645,-7.65460205458247,
8.67361737988404E-18));
#12136=CARTESIAN_POINT('Ctrl Pts',(-0.163949010525728,-7.64897891675118,
1.35275947821813E-17));
#12137=CARTESIAN_POINT('Ctrl Pts',(-0.171117084588845,-7.64300974124484,
7.79481809193044E-17));
#12138=CARTESIAN_POINT('Ctrl Pts',(-0.178013579433405,-7.63671391029203,
9.36750677027476E-17));
#12139=CARTESIAN_POINT('Ctrl Pts',(-0.181540539144798,-7.63349413812939,
1.01718007967481E-16));
#12140=CARTESIAN_POINT('Ctrl Pts',(-0.184990139201544,-7.63019455138719,
-3.81961123697981E-17));
#12141=CARTESIAN_POINT('Ctrl Pts',(-0.188356661978096,-7.6268214388693,
-3.38271077815477E-17));
#12142=CARTESIAN_POINT('Ctrl Pts',(-0.200715886255777,-7.61443802224343,
-1.77875586204687E-17));
#12143=CARTESIAN_POINT('Ctrl Pts',(-0.211972714988144,-7.60105293520862,
2.70635579723243E-17));
#12144=CARTESIAN_POINT('Ctrl Pts',(-0.221976934246241,-7.58681399582591,
-1.73472347597681E-18));
#12145=CARTESIAN_POINT('Ctrl Pts',(-0.228265887851312,-7.57786296957857,
-1.98381907493045E-17));
#12146=CARTESIAN_POINT('Ctrl Pts',(-0.234059032429037,-7.56857391909213,
2.8705858906042E-18));
#12147=CARTESIAN_POINT('Ctrl Pts',(-0.239308868459768,-7.55898027773993,
-3.46944695195361E-18));
#12148=CARTESIAN_POINT('Ctrl Pts',(-0.241553631081729,-7.55487815961855,
-6.18036376224402E-18));
#12149=CARTESIAN_POINT('Ctrl Pts',(-0.243698951449468,-7.55072033678723,
4.51101226057749E-17));
#12150=CARTESIAN_POINT('Ctrl Pts',(-0.245740602454379,-7.54650938813658,
4.85722573273506E-17));
#12151=CARTESIAN_POINT('Ctrl Pts',(-0.247686917822847,-7.54249507126515,
5.1872726408548E-17));
#12152=CARTESIAN_POINT('Ctrl Pts',(-0.249535103186422,-7.53844047081111,
8.10072286248015E-17));
#12153=CARTESIAN_POINT('Ctrl Pts',(-0.251281761611404,-7.53435006699437,
7.45931094670027E-17));
#12154=CARTESIAN_POINT('Ctrl Pts',(-0.2575376047831,-7.51969985008849,5.16202585868036E-17));
#12155=CARTESIAN_POINT('Ctrl Pts',(-0.262498407735628,-7.5045827269486,
3.19807068830928E-17));
#12156=CARTESIAN_POINT('Ctrl Pts',(-0.266024752279042,-7.4891086692212,
5.55111512312578E-17));
#12157=CARTESIAN_POINT('Ctrl Pts',(-0.268541669693304,-7.47806410880349,
6.90752738671573E-17));
#12158=CARTESIAN_POINT('Ctrl Pts',(-0.270326748263048,-7.46683731032382,
1.98990298923518E-18));
#12159=CARTESIAN_POINT('Ctrl Pts',(-0.271391863481061,-7.4554970632839,
0.));
#12160=CARTESIAN_POINT('Ctrl Pts',(-0.271805184633354,-7.45109644643555,
-7.72187818324019E-19));
#12161=CARTESIAN_POINT('Ctrl Pts',(-0.272109983012601,-7.44667877563548,
3.18736603349747E-17));
#12162=CARTESIAN_POINT('Ctrl Pts',(-0.272306561259532,-7.44224822959102,
3.12250225675825E-17));
#12163=CARTESIAN_POINT('Ctrl Pts',(-0.272509061253092,-7.43768421724747,
3.05568451584854E-17));
#12164=CARTESIAN_POINT('Ctrl Pts',(-0.27259626110233,-7.43311633646646,
7.03447662139463E-17));
#12165=CARTESIAN_POINT('Ctrl Pts',(-0.272569835270061,-7.42855113569005,
7.28583859910259E-17));
#12166=CARTESIAN_POINT('Ctrl Pts',(-0.272471756407933,-7.41160749913858,
8.21876273579062E-17));
#12167=CARTESIAN_POINT('Ctrl Pts',(-0.270813099881604,-7.39468986571343,
2.72914138058113E-17));
#12168=CARTESIAN_POINT('Ctrl Pts',(-0.267648465653111,-7.37802926095779,
-1.73472347597681E-17));
#12169=CARTESIAN_POINT('Ctrl Pts',(-0.265994330828014,-7.36932086543916,
-4.06795815039127E-17));
#12170=CARTESIAN_POINT('Ctrl Pts',(-0.263927841897732,-7.36068292366611,
3.71040643002486E-17));
#12171=CARTESIAN_POINT('Ctrl Pts',(-0.261451406717338,-7.35215143569316,
5.20417042793042E-17));
#12172=CARTESIAN_POINT('Ctrl Pts',(-0.260001090669275,-7.34715499806419,
6.07898835788593E-17));
#12173=CARTESIAN_POINT('Ctrl Pts',(-0.25840951525882,-7.34219346234189,
1.85022084656224E-17));
#12174=CARTESIAN_POINT('Ctrl Pts',(-0.256678509151567,-7.33727981648105,
2.42861286636753E-17));
#12175=CARTESIAN_POINT('Ctrl Pts',(-0.251357961519984,-7.32217687332112,
4.20640110073944E-17));
#12176=CARTESIAN_POINT('Ctrl Pts',(-0.244748745096942,-7.30759378918613,
6.42002344202532E-17));
#12177=CARTESIAN_POINT('Ctrl Pts',(-0.236874436022921,-7.29374513935771,
2.77555756156289E-17));
#12178=CARTESIAN_POINT('Ctrl Pts',(-0.23280784441881,-7.28659317178936,
8.9341727323557E-18));
#12179=CARTESIAN_POINT('Ctrl Pts',(-0.228399168283279,-7.27963277931266,
6.23483830602166E-17));
#12180=CARTESIAN_POINT('Ctrl Pts',(-0.223669100108808,-7.27292514415603,
4.16333634234434E-17));
#12181=CARTESIAN_POINT('Ctrl Pts',(-0.216422974570852,-7.2626495276924,
9.89943755332752E-18));
#12182=CARTESIAN_POINT('Ctrl Pts',(-0.208418205701992,-7.25295421133118,
-3.20573011646789E-17));
#12183=CARTESIAN_POINT('Ctrl Pts',(-0.199658657126578,-7.24395737740928,
-3.46944695195361E-17));
#12184=CARTESIAN_POINT('Ctrl Pts',(-0.197072119679919,-7.24130077385944,
-2.85083271403733E-17));
#12185=CARTESIAN_POINT('Ctrl Pts',(-0.194419679127491,-7.23870521167385,
-2.14915623890787E-17));
#12186=CARTESIAN_POINT('Ctrl Pts',(-0.1917040502342,-7.23617187785139,-2.08166817117217E-17));
#12187=CARTESIAN_POINT('Origin',(0.,0.,-0.8));
#12188=CARTESIAN_POINT('',(-8.2,-1.00421037530083E-15,-0.8));
#12189=CARTESIAN_POINT('Origin',(0.,0.,-0.8));
#12190=CARTESIAN_POINT('',(-3.5,-4.28626379701574E-16,-0.8));
#12191=CARTESIAN_POINT('Origin',(0.,0.,-0.8));
#12192=CARTESIAN_POINT('Ctrl Pts',(-0.191346599666504,7.5635987203375,-0.8));
#12193=CARTESIAN_POINT('Ctrl Pts',(-0.20250980500676,7.55310804846915,-0.8));
#12194=CARTESIAN_POINT('Ctrl Pts',(-0.212570003446807,7.5415867670429,-0.8));
#12195=CARTESIAN_POINT('Ctrl Pts',(-0.221522262311368,7.52925237897662,
-0.8));
#12196=CARTESIAN_POINT('Ctrl Pts',(-0.229528852882395,7.51822092907276,
-0.8));
#12197=CARTESIAN_POINT('Ctrl Pts',(-0.236649236537895,7.50653775609482,
-0.8));
#12198=CARTESIAN_POINT('Ctrl Pts',(-0.242860462351933,7.49433095521787,
-0.8));
#12199=CARTESIAN_POINT('Ctrl Pts',(-0.244940827324234,7.49024245453724,
-0.8));
#12200=CARTESIAN_POINT('Ctrl Pts',(-0.24691968074903,7.48609356366845,-0.8));
#12201=CARTESIAN_POINT('Ctrl Pts',(-0.248793536546706,7.48189328763567,
-0.8));
#12202=CARTESIAN_POINT('Ctrl Pts',(-0.255493735434215,7.46687469077406,
-0.8));
#12203=CARTESIAN_POINT('Ctrl Pts',(-0.260811047538467,7.45130199730205,
-0.8));
#12204=CARTESIAN_POINT('Ctrl Pts',(-0.264722764385489,7.43540128965534,
-0.8));
#12205=CARTESIAN_POINT('Ctrl Pts',(-0.267427485323018,7.42440689037352,
-0.8));
#12206=CARTESIAN_POINT('Ctrl Pts',(-0.269459531552823,7.41325460272601,
-0.8));
#12207=CARTESIAN_POINT('Ctrl Pts',(-0.270799571424799,7.40201084264177,
-0.8));
#12208=CARTESIAN_POINT('Ctrl Pts',(-0.271554526921096,7.39567630092241,
-0.8));
#12209=CARTESIAN_POINT('Ctrl Pts',(-0.272089651581207,7.38931263212047,
-0.8));
#12210=CARTESIAN_POINT('Ctrl Pts',(-0.272399894416452,7.38293128541091,
-0.8));
#12211=CARTESIAN_POINT('Ctrl Pts',(-0.272610151901875,7.37860652506082,
-0.8));
#12212=CARTESIAN_POINT('Ctrl Pts',(-0.272716621945222,7.37428271302943,
-0.8));
#12213=CARTESIAN_POINT('Ctrl Pts',(-0.27271881100291,7.36996531010121,-0.8));
#12214=CARTESIAN_POINT('Ctrl Pts',(-0.272726804747392,7.35419952374042,
-0.8));
#12215=CARTESIAN_POINT('Ctrl Pts',(-0.271347453373968,7.33851305838944,
-0.8));
#12216=CARTESIAN_POINT('Ctrl Pts',(-0.268537997639155,7.32308171994473,
-0.8));
#12217=CARTESIAN_POINT('Ctrl Pts',(-0.266219513087219,7.31034711111768,
-0.8));
#12218=CARTESIAN_POINT('Ctrl Pts',(-0.262926612476523,7.29778555143682,
-0.8));
#12219=CARTESIAN_POINT('Ctrl Pts',(-0.258732497897385,7.28546433529152,
-0.8));
#12220=CARTESIAN_POINT('Ctrl Pts',(-0.256787665913683,7.27975092551567,
-0.8));
#12221=CARTESIAN_POINT('Ctrl Pts',(-0.254646751184067,7.27408525256649,
-0.8));
#12222=CARTESIAN_POINT('Ctrl Pts',(-0.252327772084624,7.26850081285998,
-0.8));
#12223=CARTESIAN_POINT('Ctrl Pts',(-0.24581334288864,7.25281311775483,-0.8));
#12224=CARTESIAN_POINT('Ctrl Pts',(-0.237886794345816,7.23772748623907,
-0.8));
#12225=CARTESIAN_POINT('Ctrl Pts',(-0.228725770337881,7.22338640333096,
-0.8));
#12226=CARTESIAN_POINT('Ctrl Pts',(-0.223374411591948,7.21500914338927,
-0.8));
#12227=CARTESIAN_POINT('Ctrl Pts',(-0.217600782266579,7.20688593688198,
-0.8));
#12228=CARTESIAN_POINT('Ctrl Pts',(-0.211432677139281,7.19904694387202,
-0.8));
#12229=CARTESIAN_POINT('Ctrl Pts',(-0.207419991121397,7.1939472549082,-0.8));
#12230=CARTESIAN_POINT('Ctrl Pts',(-0.203240245884041,7.18896788562565,
-0.8));
#12231=CARTESIAN_POINT('Ctrl Pts',(-0.198900022769198,7.1841177635399,-0.8));
#12232=CARTESIAN_POINT('Ctrl Pts',(-0.195670399400898,7.18050871690502,
-0.8));
#12233=CARTESIAN_POINT('Ctrl Pts',(-0.192354627608631,7.17697448367564,
-0.8));
#12234=CARTESIAN_POINT('Ctrl Pts',(-0.188961560346599,7.17352409745826,
-0.8));
#12235=CARTESIAN_POINT('Ctrl Pts',(-0.179751438686603,7.16415838956568,
-0.8));
#12236=CARTESIAN_POINT('Ctrl Pts',(-0.169961157096887,7.15539686266801,
-0.8));
#12237=CARTESIAN_POINT('Ctrl Pts',(-0.159654072168358,7.14730669411858,
-0.8));
#12238=CARTESIAN_POINT('Ctrl Pts',(-0.154924675023346,7.14359452716685,
-0.8));
#12239=CARTESIAN_POINT('Ctrl Pts',(-0.150086289122297,7.14002380910476,
-0.8));
#12240=CARTESIAN_POINT('Ctrl Pts',(-0.145144207522002,7.13660166676285,
-0.8));
#12241=CARTESIAN_POINT('Ctrl Pts',(-0.139981536349868,7.13302677726397,
-0.8));
#12242=CARTESIAN_POINT('Ctrl Pts',(-0.13471214767354,7.1296186339709,-0.8));
#12243=CARTESIAN_POINT('Ctrl Pts',(-0.129347728154467,7.12638746410443,
-0.8));
#12244=CARTESIAN_POINT('Ctrl Pts',(-0.11740562697242,7.11919433587414,-0.8));
#12245=CARTESIAN_POINT('Ctrl Pts',(-0.104986064106116,7.11287221540064,
-0.8));
#12246=CARTESIAN_POINT('Ctrl Pts',(-0.0921568111370747,7.10750684175833,
-0.8));
#12247=CARTESIAN_POINT('Ctrl Pts',(-0.088006704056484,7.10577120873303,
-0.8));
#12248=CARTESIAN_POINT('Ctrl Pts',(-0.0838136309060128,7.10413580458697,
-0.8));
#12249=CARTESIAN_POINT('Ctrl Pts',(-0.0795809384672947,7.10259970795555,
-0.8));
#12250=CARTESIAN_POINT('Ctrl Pts',(0.0793799282532802,7.10307770462543,
-0.8));
#12251=CARTESIAN_POINT('Ctrl Pts',(0.0961911602327611,7.10922732837881,
-0.8));
#12252=CARTESIAN_POINT('Ctrl Pts',(0.112330857379334,7.11692876061935,-0.8));
#12253=CARTESIAN_POINT('Ctrl Pts',(0.127669412008062,7.12599976803891,-0.8));
#12254=CARTESIAN_POINT('Ctrl Pts',(0.137645134844041,7.13189927148307,-0.8));
#12255=CARTESIAN_POINT('Ctrl Pts',(0.14728154433848,7.13837917234721,-0.8));
#12256=CARTESIAN_POINT('Ctrl Pts',(0.156535364142904,7.14539796150249,-0.8));
#12257=CARTESIAN_POINT('Ctrl Pts',(0.163949176913172,7.1510211516846,-0.8));
#12258=CARTESIAN_POINT('Ctrl Pts',(0.171117322384025,7.15699038584565,-0.8));
#12259=CARTESIAN_POINT('Ctrl Pts',(0.178013882658357,7.16328628151714,-0.8));
#12260=CARTESIAN_POINT('Ctrl Pts',(0.181540759565318,7.16650598063802,-0.8));
#12261=CARTESIAN_POINT('Ctrl Pts',(0.184990279464215,7.16980548981786,-0.8));
#12262=CARTESIAN_POINT('Ctrl Pts',(0.188356726173562,7.17317852169621,-0.8));
#12263=CARTESIAN_POINT('Ctrl Pts',(0.200715946303584,7.18556191792655,-0.8));
#12264=CARTESIAN_POINT('Ctrl Pts',(0.211972771450931,7.19894698292655,-0.8));
#12265=CARTESIAN_POINT('Ctrl Pts',(0.221976987368764,7.21318590122467,-0.8));
#12266=CARTESIAN_POINT('Ctrl Pts',(0.228265932818091,7.22213690559821,-0.8));
#12267=CARTESIAN_POINT('Ctrl Pts',(0.234059070290878,7.231425933934,-0.8));
#12268=CARTESIAN_POINT('Ctrl Pts',(0.239308900334691,7.24101955361731,-0.8));
#12269=CARTESIAN_POINT('Ctrl Pts',(0.241553661905442,7.24512166523041,-0.8));
#12270=CARTESIAN_POINT('Ctrl Pts',(0.243698981293207,7.24927948171673,-0.8));
#12271=CARTESIAN_POINT('Ctrl Pts',(0.245740631388171,7.25349042424184,-0.8));
#12272=CARTESIAN_POINT('Ctrl Pts',(0.247686947093964,7.25750473775864,-0.8));
#12273=CARTESIAN_POINT('Ctrl Pts',(0.249535132735624,7.26155933511193,-0.8));
#12274=CARTESIAN_POINT('Ctrl Pts',(0.251281791380746,7.26564973614279,-0.8));
#12275=CARTESIAN_POINT('Ctrl Pts',(0.257537634638496,7.2802999414258,-0.8));
#12276=CARTESIAN_POINT('Ctrl Pts',(0.262498437191553,7.29541705678458,-0.8));
#12277=CARTESIAN_POINT('Ctrl Pts',(0.266024780552404,7.31089111260971,-0.8));
#12278=CARTESIAN_POINT('Ctrl Pts',(0.268541696557213,7.32193566918861,-0.8));
#12279=CARTESIAN_POINT('Ctrl Pts',(0.270326773646181,7.33316246674896,-0.8));
#12280=CARTESIAN_POINT('Ctrl Pts',(0.271391887422382,7.34450271522912,-0.8));
#12281=CARTESIAN_POINT('Ctrl Pts',(0.271805207529464,7.348903327465,-0.8));
#12282=CARTESIAN_POINT('Ctrl Pts',(0.272110005124503,7.353320993968,-0.8));
#12283=CARTESIAN_POINT('Ctrl Pts',(0.272306582854207,7.35775153601331,-0.8));
#12284=CARTESIAN_POINT('Ctrl Pts',(0.272509082926936,7.36231555803023,-0.8));
#12285=CARTESIAN_POINT('Ctrl Pts',(0.272596282445522,7.3668834489416,-0.8));
#12286=CARTESIAN_POINT('Ctrl Pts',(0.272569855883151,7.37144866009378,-0.8));
#12287=CARTESIAN_POINT('Ctrl Pts',(0.27247177445576,7.3883923101935,-0.8));
#12288=CARTESIAN_POINT('Ctrl Pts',(0.27081311450216,7.40530996127497,-0.8));
#12289=CARTESIAN_POINT('Ctrl Pts',(0.267648476420034,7.42197058557661,-0.8));
#12290=CARTESIAN_POINT('Ctrl Pts',(0.265994356074714,7.43067890447688,-0.8));
#12291=CARTESIAN_POINT('Ctrl Pts',(0.263927889725214,7.43931677154928,-0.8));
#12292=CARTESIAN_POINT('Ctrl Pts',(0.261451485232966,7.447848187512,-0.8));
#12293=CARTESIAN_POINT('Ctrl Pts',(0.260001161760158,7.45284467046369,-0.8));
#12294=CARTESIAN_POINT('Ctrl Pts',(0.258409576835351,7.45780625101157,-0.8));
#12295=CARTESIAN_POINT('Ctrl Pts',(0.256678558962749,7.46271994144919,-0.8));
#12296=CARTESIAN_POINT('Ctrl Pts',(0.251358016236622,7.47782290504656,-0.8));
#12297=CARTESIAN_POINT('Ctrl Pts',(0.244748805012871,7.49240601029322,-0.8));
#12298=CARTESIAN_POINT('Ctrl Pts',(0.23687450191739,7.50625468017588,-0.8));
#12299=CARTESIAN_POINT('Ctrl Pts',(0.232807882388933,7.51340671264214,-0.8));
#12300=CARTESIAN_POINT('Ctrl Pts',(0.228399173295155,7.5203671668612,-0.8));
#12301=CARTESIAN_POINT('Ctrl Pts',(0.223669067490228,7.5270748591468,-0.8));
#12302=CARTESIAN_POINT('Ctrl Pts',(0.216422943591704,7.53735047905449,-0.8));
#12303=CARTESIAN_POINT('Ctrl Pts',(0.208418177836147,7.5470457976146,-0.8));
#12304=CARTESIAN_POINT('Ctrl Pts',(0.199658634031892,7.55604263170521,-0.8));
#12305=CARTESIAN_POINT('Ctrl Pts',(0.197072096223501,7.55869923712339,-0.8));
#12306=CARTESIAN_POINT('Ctrl Pts',(0.19441965536406,7.56129480091647,-0.8));
#12307=CARTESIAN_POINT('Ctrl Pts',(0.191704026215795,7.56382813610289,-0.8));
#12308=CARTESIAN_POINT('Ctrl Pts',(7.2086534003335,0.163598720337496,-0.8));
#12309=CARTESIAN_POINT('Ctrl Pts',(7.19749017953724,0.153108033944298,-0.8));
#12310=CARTESIAN_POINT('Ctrl Pts',(7.18742996379988,0.141586740347201,-0.8));
#12311=CARTESIAN_POINT('Ctrl Pts',(7.17847768761626,0.129252341488054,-0.8));
#12312=CARTESIAN_POINT('Ctrl Pts',(7.1704711491364,0.118220975043782,-0.8));
#12313=CARTESIAN_POINT('Ctrl Pts',(7.1633508026162,0.106537897602213,-0.8));
#12314=CARTESIAN_POINT('Ctrl Pts',(7.15713959961044,0.0943312004660431,
-0.8));
#12315=CARTESIAN_POINT('Ctrl Pts',(7.15505920883279,0.0902426688041016,
-0.8));
#12316=CARTESIAN_POINT('Ctrl Pts',(7.15308033132025,0.0860937460975511,
-0.8));
#12317=CARTESIAN_POINT('Ctrl Pts',(7.1512064530744,0.0818934370748483,-0.8));
#12318=CARTESIAN_POINT('Ctrl Pts',(7.14450623072875,0.0668748495893196,
-0.8));
#12319=CARTESIAN_POINT('Ctrl Pts',(7.13918889541544,0.0513021658152235,
-0.8));
#12320=CARTESIAN_POINT('Ctrl Pts',(7.13527715751009,0.0354014666253399,
-0.8));
#12321=CARTESIAN_POINT('Ctrl Pts',(7.13257241583995,0.024407048102453,-0.8));
#12322=CARTESIAN_POINT('Ctrl Pts',(7.13054035296786,0.0132547399032318,
-0.8));
#12323=CARTESIAN_POINT('Ctrl Pts',(7.1292003013188,0.00201095788328195,
-0.8));
#12324=CARTESIAN_POINT('Ctrl Pts',(7.1284453491983,-0.00432351219812528,
-0.8));
#12325=CARTESIAN_POINT('Ctrl Pts',(7.12791022363301,-0.010687109030267,
-0.8));
#12326=CARTESIAN_POINT('Ctrl Pts',(7.1275999755608,-0.017068383912153,-0.8));
#12327=CARTESIAN_POINT('Ctrl Pts',(7.12738970979551,-0.0213931928851633,
-0.8));
#12328=CARTESIAN_POINT('Ctrl Pts',(7.12728323414032,-0.0257170542882299,
-0.8));
#12329=CARTESIAN_POINT('Ctrl Pts',(7.12728104222802,-0.0300345064165335,
-0.8));
#12330=CARTESIAN_POINT('Ctrl Pts',(7.12727303815211,-0.0458002898456707,
-0.8));
#12331=CARTESIAN_POINT('Ctrl Pts',(7.12865238357099,-0.0614867553087103,
-0.8));
#12332=CARTESIAN_POINT('Ctrl Pts',(7.1314618393697,-0.0769180982948808,
-0.8));
#12333=CARTESIAN_POINT('Ctrl Pts',(7.13378032243542,-0.0896527024168026,
-0.8));
#12334=CARTESIAN_POINT('Ctrl Pts',(7.13707322436504,-0.102214260636911,
-0.8));
#12335=CARTESIAN_POINT('Ctrl Pts',(7.14126734236948,-0.11453547787408,-0.8));
#12336=CARTESIAN_POINT('Ctrl Pts',(7.14321217687778,-0.120248890906726,
-0.8));
#12337=CARTESIAN_POINT('Ctrl Pts',(7.14535309477846,-0.125914567622866,
-0.8));
#12338=CARTESIAN_POINT('Ctrl Pts',(7.14767207759612,-0.131499011499717,
-0.8));
#12339=CARTESIAN_POINT('Ctrl Pts',(7.15418651087584,-0.147186703000945,
-0.8));
#12340=CARTESIAN_POINT('Ctrl Pts',(7.1621130650536,-0.162272335255616,-0.8));
#12341=CARTESIAN_POINT('Ctrl Pts',(7.17127409496857,-0.176613421933616,
-0.8));
#12342=CARTESIAN_POINT('Ctrl Pts',(7.17662545225571,-0.184990676392116,
-0.8));
#12343=CARTESIAN_POINT('Ctrl Pts',(7.18239907944199,-0.193113878919975,
-0.8));
#12344=CARTESIAN_POINT('Ctrl Pts',(7.18856718156875,-0.200952869302734,
-0.8));
#12345=CARTESIAN_POINT('Ctrl Pts',(7.19257981371173,-0.206052490569052,
-0.8));
#12346=CARTESIAN_POINT('Ctrl Pts',(7.19675950038746,-0.211031795839324,
-0.8));
#12347=CARTESIAN_POINT('Ctrl Pts',(7.20109966044925,-0.215881857912704,
-0.8));
#12348=CARTESIAN_POINT('Ctrl Pts',(7.2043291925446,-0.219490810326305,-0.8));
#12349=CARTESIAN_POINT('Ctrl Pts',(7.20764486889344,-0.22302495434415,-0.8));
#12350=CARTESIAN_POINT('Ctrl Pts',(7.21103783632041,-0.226475256026996,
-0.8));
#12351=CARTESIAN_POINT('Ctrl Pts',(7.22024789111854,-0.235840942038731,
-0.8));
#12352=CARTESIAN_POINT('Ctrl Pts',(7.23003810005691,-0.244602455651909,
-0.8));
#12353=CARTESIAN_POINT('Ctrl Pts',(7.24034510674114,-0.252692620249968,
-0.8));
#12354=CARTESIAN_POINT('Ctrl Pts',(7.24507777505305,-0.256407381169837,
-0.8));
#12355=CARTESIAN_POINT('Ctrl Pts',(7.24991958336186,-0.2599804973403,-0.8));
#12356=CARTESIAN_POINT('Ctrl Pts',(7.25486522766478,-0.263404826892334,
-0.8));
#12357=CARTESIAN_POINT('Ctrl Pts',(7.26002526592285,-0.266977601320589,
-0.8));
#12358=CARTESIAN_POINT('Ctrl Pts',(7.26529188355138,-0.270383791071441,
-0.8));
#12359=CARTESIAN_POINT('Ctrl Pts',(7.27065343703401,-0.27361320247099,-0.8));
#12360=CARTESIAN_POINT('Ctrl Pts',(7.28259519346882,-0.280806051425342,
-0.8));
#12361=CARTESIAN_POINT('Ctrl Pts',(7.29501437679438,-0.287127944728029,
-0.8));
#12362=CARTESIAN_POINT('Ctrl Pts',(7.30784322140636,-0.292493150612868,
-0.8));
#12363=CARTESIAN_POINT('Ctrl Pts',(7.31199333041977,-0.294228785424493,
-0.8));
#12364=CARTESIAN_POINT('Ctrl Pts',(7.3161864052494,-0.295864191114811,-0.8));
#12365=CARTESIAN_POINT('Ctrl Pts',(7.32041909912987,-0.297400289065613,
-0.8));
#12366=CARTESIAN_POINT('Ctrl Pts',(7.47937992825329,-0.29692229537457,-0.8));
#12367=CARTESIAN_POINT('Ctrl Pts',(7.49619115357747,-0.290772674055728,
-0.8));
#12368=CARTESIAN_POINT('Ctrl Pts',(7.5123308439229,-0.283071241089594,-0.8));
#12369=CARTESIAN_POINT('Ctrl Pts',(7.52766939202587,-0.27400023114592,-0.8));
#12370=CARTESIAN_POINT('Ctrl Pts',(7.53764510229467,-0.268100730982278,
-0.8));
#12371=CARTESIAN_POINT('Ctrl Pts',(7.54728149990377,-0.261620833603991,
-0.8));
#12372=CARTESIAN_POINT('Ctrl Pts',(7.55653530874326,-0.254602048410521,
-0.8));
#12373=CARTESIAN_POINT('Ctrl Pts',(7.56394907438075,-0.248978890488539,
-0.8));
#12374=CARTESIAN_POINT('Ctrl Pts',(7.57111717584829,-0.24300969247227,-0.8));
#12375=CARTESIAN_POINT('Ctrl Pts',(7.57801369580309,-0.236713836682386,
-0.8));
#12376=CARTESIAN_POINT('Ctrl Pts',(7.58154062373583,-0.233494092551808,
-0.8));
#12377=CARTESIAN_POINT('Ctrl Pts',(7.58499019302965,-0.230194535576604,
-0.8));
#12378=CARTESIAN_POINT('Ctrl Pts',(7.58835668661318,-0.226821454006683,
-0.8));
#12379=CARTESIAN_POINT('Ctrl Pts',(7.60071590929916,-0.214438045208707,
-0.8));
#12380=CARTESIAN_POINT('Ctrl Pts',(7.61197273665574,-0.201052966631013,
-0.8));
#12381=CARTESIAN_POINT('Ctrl Pts',(7.62197695463197,-0.186814035340863,
-0.8));
#12382=CARTESIAN_POINT('Ctrl Pts',(7.62826590510742,-0.177863017488208,
-0.8));
#12383=CARTESIAN_POINT('Ctrl Pts',(7.63405904695874,-0.16857397550271,-0.8));
#12384=CARTESIAN_POINT('Ctrl Pts',(7.63930888069208,-0.158980342466583,
-0.8));
#12385=CARTESIAN_POINT('Ctrl Pts',(7.64155364292289,-0.154878226820711,
-0.8));
#12386=CARTESIAN_POINT('Ctrl Pts',(7.64369896292573,-0.150720406401628,
-0.8));
#12387=CARTESIAN_POINT('Ctrl Pts',(7.64574061359146,-0.146509460078439,
-0.8));
#12388=CARTESIAN_POINT('Ctrl Pts',(7.64768692907881,-0.142495144513688,
-0.8));
#12389=CARTESIAN_POINT('Ctrl Pts',(7.64953511453937,-0.138440545269517,
-0.8));
#12390=CARTESIAN_POINT('Ctrl Pts',(7.65128177304014,-0.134350142542067,
-0.8));
#12391=CARTESIAN_POINT('Ctrl Pts',(7.65753761624241,-0.119699930101675,
-0.8));
#12392=CARTESIAN_POINT('Ctrl Pts',(7.66249841903988,-0.104582809953302,
-0.8));
#12393=CARTESIAN_POINT('Ctrl Pts',(7.66602476312854,-0.0891087529615867,
-0.8));
#12394=CARTESIAN_POINT('Ctrl Pts',(7.668541680002,-0.0780641940177735,-0.8));
#12395=CARTESIAN_POINT('Ctrl Pts',(7.67032675800354,-0.0668373958916314,
-0.8));
#12396=CARTESIAN_POINT('Ctrl Pts',(7.67139187266829,-0.0554971482997141,
-0.8));
#12397=CARTESIAN_POINT('Ctrl Pts',(7.67180519341954,-0.051096533221107,
-0.8));
#12398=CARTESIAN_POINT('Ctrl Pts',(7.67210999149788,-0.046678864069736,
-0.8));
#12399=CARTESIAN_POINT('Ctrl Pts',(7.67230656954632,-0.0422483195596408,
-0.8));
#12400=CARTESIAN_POINT('Ctrl Pts',(7.67250906957021,-0.0376843035048666,
-0.8));
#12401=CARTESIAN_POINT('Ctrl Pts',(7.67259626929253,-0.0331164188372603,
-0.8));
#12402=CARTESIAN_POINT('Ctrl Pts',(7.67256984318009,-0.0285512140800657,
-0.8));
#12403=CARTESIAN_POINT('Ctrl Pts',(7.67247176333353,-0.0116075723308694,
-0.8));
#12404=CARTESIAN_POINT('Ctrl Pts',(7.67081310549201,0.00531006786860519,
-0.8));
#12405=CARTESIAN_POINT('Ctrl Pts',(7.66764846978472,0.0219706801239459,
-0.8));
#12406=CARTESIAN_POINT('Ctrl Pts',(7.66599434051542,0.030679046244134,-0.8));
#12407=CARTESIAN_POINT('Ctrl Pts',(7.66392786024929,0.0393169593546687,
-0.8));
#12408=CARTESIAN_POINT('Ctrl Pts',(7.66145143684384,0.0478484196974881,
-0.8));
#12409=CARTESIAN_POINT('Ctrl Pts',(7.66000111794769,0.0528448747139515,
-0.8));
#12410=CARTESIAN_POINT('Ctrl Pts',(7.65840953888752,0.0578064276330517,
-0.8));
#12411=CARTESIAN_POINT('Ctrl Pts',(7.65667852826701,0.0627200905953307,
-0.8));
#12412=CARTESIAN_POINT('Ctrl Pts',(7.65135798251779,0.0778230415981986,
-0.8));
#12413=CARTESIAN_POINT('Ctrl Pts',(7.64474876808975,0.0924061338350732,
-0.8));
#12414=CARTESIAN_POINT('Ctrl Pts',(7.63687446130966,0.106254791359862,-0.8));
#12415=CARTESIAN_POINT('Ctrl Pts',(7.63280785898707,0.113406783837146,-0.8));
#12416=CARTESIAN_POINT('Ctrl Pts',(7.62839917020088,0.120367200011687,-0.8));
#12417=CARTESIAN_POINT('Ctrl Pts',(7.62366908758241,0.127074857095534,-0.8));
#12418=CARTESIAN_POINT('Ctrl Pts',(7.61642296267604,0.137350474876241,-0.8));
#12419=CARTESIAN_POINT('Ctrl Pts',(7.60841819500501,0.147045792077381,-0.8));
#12420=CARTESIAN_POINT('Ctrl Pts',(7.59965864826425,0.156042626060984,-0.8));
#12421=CARTESIAN_POINT('Ctrl Pts',(7.59707211067876,0.158699230328034,-0.8));
#12422=CARTESIAN_POINT('Ctrl Pts',(7.59441967000851,0.161294793130762,-0.8));
#12423=CARTESIAN_POINT('Ctrl Pts',(7.59170404101736,0.163828127476924,-0.8));
#12424=CARTESIAN_POINT('Ctrl Pts',(-7.59134659966651,0.163598720337494,
-0.8));
#12425=CARTESIAN_POINT('Ctrl Pts',(-7.60250980500677,0.153108048469134,
-0.8));
#12426=CARTESIAN_POINT('Ctrl Pts',(-7.61257000344682,0.141586767042882,
-0.8));
#12427=CARTESIAN_POINT('Ctrl Pts',(-7.62152226231139,0.129252378976592,
-0.8));
#12428=CARTESIAN_POINT('Ctrl Pts',(-7.62952885288343,0.118220929071331,
-0.8));
#12429=CARTESIAN_POINT('Ctrl Pts',(-7.63664923653971,0.106537756091835,
-0.8));
#12430=CARTESIAN_POINT('Ctrl Pts',(-7.6428604623543,0.0943309552132166,
-0.8));
#12431=CARTESIAN_POINT('Ctrl Pts',(-7.6449408273248,0.0902424545359381,
-0.8));
#12432=CARTESIAN_POINT('Ctrl Pts',(-7.64691968074795,0.0860935636706147,
-0.8));
#12433=CARTESIAN_POINT('Ctrl Pts',(-7.64879353654417,0.0818932876413604,
-0.8));
#12434=CARTESIAN_POINT('Ctrl Pts',(-7.65549373543205,0.0668746907798337,
-0.799999999999999));
#12435=CARTESIAN_POINT('Ctrl Pts',(-7.66081104753667,0.0513019973078679,
-0.8));
#12436=CARTESIAN_POINT('Ctrl Pts',(-7.66472276438405,0.0354012896611767,
-0.8));
#12437=CARTESIAN_POINT('Ctrl Pts',(-7.6674274853223,0.0244068903774662,
-0.8));
#12438=CARTESIAN_POINT('Ctrl Pts',(-7.66945953155259,0.0132546027280042,
-0.8));
#12439=CARTESIAN_POINT('Ctrl Pts',(-7.6707995714248,0.00201084264178555,
-0.8));
#12440=CARTESIAN_POINT('Ctrl Pts',(-7.67155452692688,-0.00432369912609444,
-0.8));
#12441=CARTESIAN_POINT('Ctrl Pts',(-7.67208965158941,-0.0106873679770006,
-0.799999999999999));
#12442=CARTESIAN_POINT('Ctrl Pts',(-7.67239989442358,-0.0170687147357037,
-0.799999999999999));
#12443=CARTESIAN_POINT('Ctrl Pts',(-7.67261015190465,-0.0213934750445532,
-0.799999999999999));
#12444=CARTESIAN_POINT('Ctrl Pts',(-7.67271662194561,-0.0257172870342268,
-0.8));
#12445=CARTESIAN_POINT('Ctrl Pts',(-7.67271881100292,-0.030034689921079,
-0.8));
#12446=CARTESIAN_POINT('Ctrl Pts',(-7.67272680474609,-0.0458004762743684,
-0.8));
#12447=CARTESIAN_POINT('Ctrl Pts',(-7.67134745337264,-0.0614869416178373,
-0.8));
#12448=CARTESIAN_POINT('Ctrl Pts',(-7.66853799763916,-0.0769182800552743,
-0.8));
#12449=CARTESIAN_POINT('Ctrl Pts',(-7.66621951308713,-0.0896528888827926,
-0.8));
#12450=CARTESIAN_POINT('Ctrl Pts',(-7.66292661247628,-0.102214448564117,
-0.8));
#12451=CARTESIAN_POINT('Ctrl Pts',(-7.65873249789692,-0.114535664709849,
-0.8));
#12452=CARTESIAN_POINT('Ctrl Pts',(-7.65678766591361,-0.120249074484433,
-0.8));
#12453=CARTESIAN_POINT('Ctrl Pts',(-7.65464675118448,-0.125914747432373,
-0.8));
#12454=CARTESIAN_POINT('Ctrl Pts',(-7.6523277720856,-0.131499187137676,
-0.8));
#12455=CARTESIAN_POINT('Ctrl Pts',(-7.64581334288988,-0.147186882242587,
-0.8));
#12456=CARTESIAN_POINT('Ctrl Pts',(-7.63788679434737,-0.162272513758134,
-0.8));
#12457=CARTESIAN_POINT('Ctrl Pts',(-7.62872577033978,-0.176613596666072,
-0.8));
#12458=CARTESIAN_POINT('Ctrl Pts',(-7.62337441159445,-0.184990856607026,
-0.8));
#12459=CARTESIAN_POINT('Ctrl Pts',(-7.61760078226976,-0.193114063113643,
-0.8));
#12460=CARTESIAN_POINT('Ctrl Pts',(-7.61143267714321,-0.200953056122988,
-0.8));
#12461=CARTESIAN_POINT('Ctrl Pts',(-7.60741999113199,-0.206052745078555,
-0.8));
#12462=CARTESIAN_POINT('Ctrl Pts',(-7.60324024590185,-0.21103211435324,
-0.8));
#12463=CARTESIAN_POINT('Ctrl Pts',(-7.59890002279473,-0.215882236431572,
-0.8));
#12464=CARTESIAN_POINT('Ctrl Pts',(-7.59567039942596,-0.21949128306788,
-0.8));
#12465=CARTESIAN_POINT('Ctrl Pts',(-7.5923546276331,-0.223025516298712,
-0.8));
#12466=CARTESIAN_POINT('Ctrl Pts',(-7.58896156037046,-0.226475902517482,
-0.8));
#12467=CARTESIAN_POINT('Ctrl Pts',(-7.57975143871387,-0.235841610408655,
-0.8));
#12468=CARTESIAN_POINT('Ctrl Pts',(-7.5699611571278,-0.244603137305301,
-0.8));
#12469=CARTESIAN_POINT('Ctrl Pts',(-7.55965407220312,-0.252693305854133,
-0.8));
#12470=CARTESIAN_POINT('Ctrl Pts',(-7.55492467495832,-0.256405472885301,
-0.8));
#12471=CARTESIAN_POINT('Ctrl Pts',(-7.55008628895285,-0.25997619102085,
-0.8));
#12472=CARTESIAN_POINT('Ctrl Pts',(-7.54514420724383,-0.263398333429773,
-0.8));
#12473=CARTESIAN_POINT('Ctrl Pts',(-7.53998153614902,-0.266973222866464,
-0.8));
#12474=CARTESIAN_POINT('Ctrl Pts',(-7.53471214755407,-0.27038136610209,
-0.8));
#12475=CARTESIAN_POINT('Ctrl Pts',(-7.52934772811915,-0.273612535916845,
-0.8));
#12476=CARTESIAN_POINT('Ctrl Pts',(-7.51740562694793,-0.280805664138331,
-0.8));
#12477=CARTESIAN_POINT('Ctrl Pts',(-7.50498606409347,-0.287127784604654,
-0.8));
#12478=CARTESIAN_POINT('Ctrl Pts',(-7.49215681113707,-0.292493158241675,
-0.8));
#12479=CARTESIAN_POINT('Ctrl Pts',(-7.48800670405648,-0.294228791266972,
-0.8));
#12480=CARTESIAN_POINT('Ctrl Pts',(-7.48381363090601,-0.295864195413031,
-0.8));
#12481=CARTESIAN_POINT('Ctrl Pts',(-7.47958093846729,-0.297400292044454,
-0.8));
#12482=CARTESIAN_POINT('Ctrl Pts',(-7.32062007174671,-0.29692229537457,
-0.8));
#12483=CARTESIAN_POINT('Ctrl Pts',(-7.30380883220412,-0.290772668854571,
-0.8));
#12484=CARTESIAN_POINT('Ctrl Pts',(-7.28766912732842,-0.283071237438702,
-0.8));
#12485=CARTESIAN_POINT('Ctrl Pts',(-7.27233056528333,-0.274000232887525,
-0.8));
#12486=CARTESIAN_POINT('Ctrl Pts',(-7.26235482816667,-0.268100725715958,
-0.8));
#12487=CARTESIAN_POINT('Ctrl Pts',(-7.25271840516627,-0.261620820891142,
-0.8));
#12488=CARTESIAN_POINT('Ctrl Pts',(-7.24346457290171,-0.254602027234289,
-0.8));
#12489=CARTESIAN_POINT('Ctrl Pts',(-7.23605070657022,-0.248978800392428,
-0.8));
#12490=CARTESIAN_POINT('Ctrl Pts',(-7.22888251109443,-0.243009525157091,
-0.8));
#12491=CARTESIAN_POINT('Ctrl Pts',(-7.22198590500135,-0.236713584164732,
-0.8));
#12492=CARTESIAN_POINT('Ctrl Pts',(-7.21845908607672,-0.233493936189985,
-0.8));
#12493=CARTESIAN_POINT('Ctrl Pts',(-7.21500962230698,-0.2301944813217,-0.8));
#12494=CARTESIAN_POINT('Ctrl Pts',(-7.21164322886242,-0.226821505909535,
-0.8));
#12495=CARTESIAN_POINT('Ctrl Pts',(-7.19928401163746,-0.214438123960911,
-0.8));
#12496=CARTESIAN_POINT('Ctrl Pts',(-7.188027189001,-0.201053074390168,-0.8));
#12497=CARTESIAN_POINT('Ctrl Pts',(-7.17802297542257,-0.186814170855175,
-0.8));
#12498=CARTESIAN_POINT('Ctrl Pts',(-7.171734035686,-0.177863181799981,-0.8));
#12499=CARTESIAN_POINT('Ctrl Pts',(-7.16594090318987,-0.168574168976251,
-0.8));
#12500=CARTESIAN_POINT('Ctrl Pts',(-7.16069107733955,-0.15898056446742,
-0.8));
#12501=CARTESIAN_POINT('Ctrl Pts',(-7.15844631652005,-0.154878457438895,
-0.8));
#12502=CARTESIAN_POINT('Ctrl Pts',(-7.15630099783232,-0.15072064542349,
-0.8));
#12503=CARTESIAN_POINT('Ctrl Pts',(-7.15425934838691,-0.146509707216243,
-0.8));
#12504=CARTESIAN_POINT('Ctrl Pts',(-7.15231303243113,-0.142495396022921,
-0.8));
#12505=CARTESIAN_POINT('Ctrl Pts',(-7.15046484658208,-0.138440800814485,
-0.8));
#12506=CARTESIAN_POINT('Ctrl Pts',(-7.14871818777149,-0.134350401707579,
-0.8));
#12507=CARTESIAN_POINT('Ctrl Pts',(-7.1424623444498,-0.119700204553552,
-0.8));
#12508=CARTESIAN_POINT('Ctrl Pts',(-7.13750154217398,-0.104583094632127,
-0.8));
#12509=CARTESIAN_POINT('Ctrl Pts',(-7.13397519964019,-0.0891090401260764,
-0.8));
#12510=CARTESIAN_POINT('Ctrl Pts',(-7.13145828462303,-0.0780644862322087,
-0.8));
#12511=CARTESIAN_POINT('Ctrl Pts',(-7.12967320857157,-0.0668376893119182,
-0.8));
#12512=CARTESIAN_POINT('Ctrl Pts',(-7.12860809580548,-0.0554974398191664,
-0.8));
#12513=CARTESIAN_POINT('Ctrl Pts',(-7.12819477643118,-0.0510968308188738,
-0.8));
#12514=CARTESIAN_POINT('Ctrl Pts',(-7.12788997938578,-0.0466791673306104,
-0.8));
#12515=CARTESIAN_POINT('Ctrl Pts',(-7.12769340201838,-0.0422486280913985,
-0.8));
#12516=CARTESIAN_POINT('Ctrl Pts',(-7.12749090188967,-0.0376845992915606,
-0.8));
#12517=CARTESIAN_POINT('Ctrl Pts',(-7.12740370260243,-0.0331167012771051,
-0.8));
#12518=CARTESIAN_POINT('Ctrl Pts',(-7.12743012967622,-0.0285514828500066,
-0.8));
#12519=CARTESIAN_POINT('Ctrl Pts',(-7.12752821290038,-0.0116078232524714,
-0.8));
#12520=CARTESIAN_POINT('Ctrl Pts',(-7.12918687525478,0.00530984020385254,
-0.8));
#12521=CARTESIAN_POINT('Ctrl Pts',(-7.13235151603647,0.021970478203028,
-0.8));
#12522=CARTESIAN_POINT('Ctrl Pts',(-7.13400562623726,0.0306787434271353,
-0.8));
#12523=CARTESIAN_POINT('Ctrl Pts',(-7.13607207676681,0.0393165581665612,
-0.8));
#12524=CARTESIAN_POINT('Ctrl Pts',(-7.13854845975925,0.0478479236807756,
-0.8));
#12525=CARTESIAN_POINT('Ctrl Pts',(-7.13999878843953,0.0528444384061105,
-0.8));
#12526=CARTESIAN_POINT('Ctrl Pts',(-7.14159038003695,0.0578060503789822,
-0.8));
#12527=CARTESIAN_POINT('Ctrl Pts',(-7.14332140616028,0.0627197720666046,
-0.8));
#12528=CARTESIAN_POINT('Ctrl Pts',(-7.1486419454519,0.0778227499793214,
-0.8));
#12529=CARTESIAN_POINT('Ctrl Pts',(-7.15525115303475,0.092405870012346,
-0.8));
#12530=CARTESIAN_POINT('Ctrl Pts',(-7.16312545194293,0.106254553939122,
-0.8));
#12531=CARTESIAN_POINT('Ctrl Pts',(-7.16719209102926,0.113406631858387,
-0.8));
#12532=CARTESIAN_POINT('Ctrl Pts',(-7.17160082320644,0.120367129319865,
-0.799999999999999));
#12533=CARTESIAN_POINT('Ctrl Pts',(-7.17633095536696,0.127074861616176,
-0.799999999999999));
#12534=CARTESIAN_POINT('Ctrl Pts',(-7.18357707811536,0.137350483931364,
-0.799999999999999));
#12535=CARTESIAN_POINT('Ctrl Pts',(-7.19158184168782,0.147045804025915,
-0.799999999999999));
#12536=CARTESIAN_POINT('Ctrl Pts',(-7.2003413821471,0.156042638227876,-0.799999999999999));
#12537=CARTESIAN_POINT('Ctrl Pts',(-7.20292792020884,0.158699244953618,
-0.799999999999999));
#12538=CARTESIAN_POINT('Ctrl Pts',(-7.20558036128329,0.161294809871419,
-0.799999999999999));
#12539=CARTESIAN_POINT('Ctrl Pts',(-7.2082959906101,0.163828146011838,-0.799999999999999));
#12540=CARTESIAN_POINT('Origin',(-7.4,0.,0.220842344717745));
#12541=CARTESIAN_POINT('Ctrl Pts',(-7.70772056490863,0.000154295167761212,
-0.0291576552822542));
#12542=CARTESIAN_POINT('Ctrl Pts',(-7.70778424817136,0.0100435505178975,
-0.0296715621794889));
#12543=CARTESIAN_POINT('Ctrl Pts',(-7.70290029244162,0.120578394498565,
-0.035418806655132));
#12544=CARTESIAN_POINT('Ctrl Pts',(-7.56952504259133,0.319794750950713,
-0.0463993887091835));
#12545=CARTESIAN_POINT('Ctrl Pts',(-7.2268011951414,0.317782806798611,-0.0620994014444089));
#12546=CARTESIAN_POINT('Ctrl Pts',(-7.03939107410859,0.0308556281233394,
-0.0777994141796342));
#12547=CARTESIAN_POINT('Ctrl Pts',(-7.17534010740672,-0.283761737281935,
-0.0934994269148595));
#12548=CARTESIAN_POINT('Ctrl Pts',(-7.51274497664259,-0.343916495026914,
-0.109199439650085));
#12549=CARTESIAN_POINT('Ctrl Pts',(-7.69164526295008,-0.155985565502471,
-0.12108551577255));
#12550=CARTESIAN_POINT('Ctrl Pts',(-7.70747663110457,-0.0276893459128193,
-0.127738254316606));
#12551=CARTESIAN_POINT('Ctrl Pts',(-7.70724559592217,-0.000260666439420156,
-0.129157655282254));
#12552=CARTESIAN_POINT('Ctrl Pts',(-7.70701976654778,-0.000306170806070059,
-0.0208423447177452));
#12553=CARTESIAN_POINT('Ctrl Pts',(-7.70655486683947,0.0677880488673211,
-0.0243615716353137));
#12554=CARTESIAN_POINT('Ctrl Pts',(-7.65102809142816,0.238050536013955,
-0.0331141361312906));
#12555=CARTESIAN_POINT('Ctrl Pts',(-7.37136424514298,0.36072194419717,-0.0471000382056761));
#12556=CARTESIAN_POINT('Ctrl Pts',(-7.0833377209053,0.175239119455976,-0.0628000509409012));
#12557=CARTESIAN_POINT('Ctrl Pts',(-7.07914899542098,-0.167517421922754,
-0.0785000636761269));
#12558=CARTESIAN_POINT('Ctrl Pts',(-7.3627280810489,-0.359992553262469,
-0.0942000764113519));
#12559=CARTESIAN_POINT('Ctrl Pts',(-7.64768205623712,-0.242854235705339,
-0.108314170091892));
#12560=CARTESIAN_POINT('Ctrl Pts',(-7.70661024184805,-0.0702887181447709,
-0.117194926194023));
#12561=CARTESIAN_POINT('Ctrl Pts',(-7.70715908192673,0.000245638898741782,
-0.120842344717745));
#12562=CARTESIAN_POINT('Ctrl Pts',(-7.20865340033349,0.163598720337495,
0.));
#12563=CARTESIAN_POINT('Ctrl Pts',(-7.15485882039215,0.100680074451818,
-0.00523333757840845));
#12564=CARTESIAN_POINT('Ctrl Pts',(-7.11504792740546,-0.081320987239729,
-0.0157000127352253));
#12565=CARTESIAN_POINT('Ctrl Pts',(-7.31088738477093,-0.282913381389853,
-0.0314000254704507));
#12566=CARTESIAN_POINT('Ctrl Pts',(-7.58669428177702,-0.230208447695885,
-0.047100038205676));
#12567=CARTESIAN_POINT('Ctrl Pts',(-7.69505959198511,0.0286321132263963,
-0.0628000509409014));
#12568=CARTESIAN_POINT('Ctrl Pts',(-7.53885775003211,0.261943479914891,
-0.0785000636761267));
#12569=CARTESIAN_POINT('Ctrl Pts',(-7.25813307589668,0.260295498980154,
-0.0942000764113521));
#12570=CARTESIAN_POINT('Ctrl Pts',(-7.10462568051681,0.0252738063447232,
-0.109900089146577));
#12571=CARTESIAN_POINT('Ctrl Pts',(-7.21598136339561,-0.232428883555319,
-0.125600101881803));
#12572=CARTESIAN_POINT('Ctrl Pts',(-7.49234926913868,-0.281701570271761,
-0.141300114617028));
#12573=CARTESIAN_POINT('Ctrl Pts',(-7.68590623015859,-0.0783741170228757,
-0.157000127352253));
#12574=CARTESIAN_POINT('Ctrl Pts',(-7.62308856437211,0.195234321246773,
-0.172700140087479));
#12575=CARTESIAN_POINT('Ctrl Pts',(-7.36022512733543,0.293773198343426,
-0.188400152822704));
#12576=CARTESIAN_POINT('Ctrl Pts',(-7.13302825740755,0.12888336190753,-0.204100165557929));
#12577=CARTESIAN_POINT('Ctrl Pts',(-7.1452274819044,-0.15157768529494,-0.219800178293155));
#12578=CARTESIAN_POINT('Ctrl Pts',(-7.38588368162235,-0.296117437159506,
-0.23550019102838));
#12579=CARTESIAN_POINT('Ctrl Pts',(-7.63919811247918,-0.175125907145724,
-0.251200203763605));
#12580=CARTESIAN_POINT('Ctrl Pts',(-7.67802130457259,0.102902736043491,
-0.266900216498831));
#12581=CARTESIAN_POINT('Ctrl Pts',(-7.46754012392463,0.288657492672429,
-0.282600229234056));
#12582=CARTESIAN_POINT('Ctrl Pts',(-7.19649506705352,0.215570314274908,
-0.298300241969282));
#12583=CARTESIAN_POINT('Ctrl Pts',(-7.10793483547166,-0.050820836942206,
-0.314000254704507));
#12584=CARTESIAN_POINT('Ctrl Pts',(-7.28127223907772,-0.271640454175529,
-0.329700267439732));
#12585=CARTESIAN_POINT('Ctrl Pts',(-7.56107396482191,-0.24887747111374,
-0.345400280174958));
#12586=CARTESIAN_POINT('Ctrl Pts',(-7.6964391210875,-0.00294367160307863,
-0.361100292910183));
#12587=CARTESIAN_POINT('Ctrl Pts',(-7.56598447354143,0.245629746235912,
-0.376800305645408));
#12588=CARTESIAN_POINT('Ctrl Pts',(-7.28668995619815,0.273944614280356,
-0.392500318380634));
#12589=CARTESIAN_POINT('Ctrl Pts',(-7.10900164217772,0.0566107185302396,
-0.408200331115859));
#12590=CARTESIAN_POINT('Ctrl Pts',(-7.19225434732208,-0.211486551584725,
-0.423900343851084));
#12591=CARTESIAN_POINT('Ctrl Pts',(-7.46179457226168,-0.289941802019968,
-0.43960035658631));
#12592=CARTESIAN_POINT('Ctrl Pts',(-7.67592301138651,-0.108403456956597,
-0.455300369321535));
#12593=CARTESIAN_POINT('Ctrl Pts',(-7.64262863919221,0.170341307842165,
-0.47100038205676));
#12594=CARTESIAN_POINT('Ctrl Pts',(-7.39176683840533,0.296339387901059,
-0.486700394791986));
#12595=CARTESIAN_POINT('Ctrl Pts',(-7.14828779291894,0.156607095511924,
-0.502400407527211));
#12596=CARTESIAN_POINT('Ctrl Pts',(-7.13052149770804,-0.12355628110687,
-0.518100420262436));
#12597=CARTESIAN_POINT('Ctrl Pts',(-7.35439916203589,-0.292925556596044,
-0.533800432997662));
#12598=CARTESIAN_POINT('Ctrl Pts',(-7.61916753267196,-0.199625672292344,
-0.549500445732886));
#12599=CARTESIAN_POINT('Ctrl Pts',(-7.68740627934318,0.0726804614431528,
-0.565200458468113));
#12600=CARTESIAN_POINT('Ctrl Pts',(-7.49792504763019,0.279813340307149,
-0.580900471203337));
#12601=CARTESIAN_POINT('Ctrl Pts',(-7.22063350732225,0.236034887969839,
-0.596600483938563));
#12602=CARTESIAN_POINT('Ctrl Pts',(-7.10418157928289,-0.0193982633392013,
-0.612300496673788));
#12603=CARTESIAN_POINT('Ctrl Pts',(-7.25299295271724,-0.257436905607251,
-0.628000509409014));
#12604=CARTESIAN_POINT('Ctrl Pts',(-7.53362678302623,-0.26462920363873,
-0.643700522144238));
#12605=CARTESIAN_POINT('Ctrl Pts',(-7.69443654339104,-0.0345263618448277,
-0.659400534879465));
#12606=CARTESIAN_POINT('Ctrl Pts',(-7.59122152812465,0.226537418199014,
-0.675100547614689));
#12607=CARTESIAN_POINT('Ctrl Pts',(-7.31653775068187,0.284461271780152,
-0.690800560349915));
#12608=CARTESIAN_POINT('Ctrl Pts',(-7.11669251625801,0.0873093018200402,
-0.70650057308514));
#12609=CARTESIAN_POINT('Ctrl Pts',(-7.17089758104745,-0.188140467543259,
-0.722200585820366));
#12610=CARTESIAN_POINT('Ctrl Pts',(-7.43052936616057,-0.294869341820571,
-0.73790059855559));
#12611=CARTESIAN_POINT('Ctrl Pts',(-7.66280860159844,-0.137213338782277,
-0.753600611290817));
#12612=CARTESIAN_POINT('Ctrl Pts',(-7.65937760170093,0.143538219530879,
-0.76930062402604));
#12613=CARTESIAN_POINT('Ctrl Pts',(-7.42345550125086,0.295466620280292,
-0.785000636761269));
#12614=CARTESIAN_POINT('Ctrl Pts',(-7.16630823828261,0.182672384524398,
-0.80070064949649));
#12615=CARTESIAN_POINT('Ctrl Pts',(-7.11910685953888,-0.0943918973400733,
-0.816400662231719));
#12616=CARTESIAN_POINT('Ctrl Pts',(-7.25500804955002,-0.221828784507026,
-0.826867337388535));
#12617=CARTESIAN_POINT('Ctrl Pts',(-7.33498000020249,-0.243208680203507,
-0.832100674966943));
#12618=CARTESIAN_POINT('Ctrl Pts',(-7.19456684496579,0.175642532122685,
0.0107002249889811));
#12619=CARTESIAN_POINT('Ctrl Pts',(-7.13681201524657,0.108091940906,0.00546688741057261));
#12620=CARTESIAN_POINT('Ctrl Pts',(-7.09407032365007,-0.0873076762705518,
-0.00499978774624428));
#12621=CARTESIAN_POINT('Ctrl Pts',(-7.30432709161405,-0.303740900761287,
-0.0206998004814696));
#12622=CARTESIAN_POINT('Ctrl Pts',(-7.60043834277246,-0.247155934874821,
-0.0363998132166949));
#12623=CARTESIAN_POINT('Ctrl Pts',(-7.71678129117659,0.0307399523464065,
-0.0520998259519203));
#12624=CARTESIAN_POINT('Ctrl Pts',(-7.54908018088519,0.281227236926832,
-0.0677998386871455));
#12625=CARTESIAN_POINT('Ctrl Pts',(-7.24768911564492,0.27945793491964,-0.0834998514223711));
#12626=CARTESIAN_POINT('Ctrl Pts',(-7.08288081171408,0.027134413604262,
-0.0991998641575962));
#12627=CARTESIAN_POINT('Ctrl Pts',(-7.20243427806597,-0.249539834797524,
-0.114899876892822));
#12628=CARTESIAN_POINT('Ctrl Pts',(-7.49914783830665,-0.302439878523479,
-0.130599889628047));
#12629=CARTESIAN_POINT('Ctrl Pts',(-7.70695407709247,-0.084143863340614,
-0.146299902363272));
#12630=CARTESIAN_POINT('Ctrl Pts',(-7.63951189992867,0.209607082930084,
-0.161999915098497));
#12631=CARTESIAN_POINT('Ctrl Pts',(-7.35729698046994,0.315400195798434,
-0.177699927833723));
#12632=CARTESIAN_POINT('Ctrl Pts',(-7.1133743297172,0.138371498183013,-0.193399940568948));
#12633=CARTESIAN_POINT('Ctrl Pts',(-7.1264716368119,-0.162736532434825,
-0.209099953304173));
#12634=CARTESIAN_POINT('Ctrl Pts',(-7.38484446639323,-0.317917012804747,
-0.224799966039399));
#12635=CARTESIAN_POINT('Ctrl Pts',(-7.6568074008656,-0.188018327453308,
-0.240499978774624));
#12636=CARTESIAN_POINT('Ctrl Pts',(-7.69848867899726,0.110478230414916,
-0.25619999150985));
#12637=CARTESIAN_POINT('Ctrl Pts',(-7.47251229325957,0.309907882070095,
-0.271900004245075));
#12638=CARTESIAN_POINT('Ctrl Pts',(-7.18151343941786,0.231440171241058,
-0.287600016980301));
#12639=CARTESIAN_POINT('Ctrl Pts',(-7.0864335800625,-0.0545621656863128,
-0.303300029715526));
#12640=CARTESIAN_POINT('Ctrl Pts',(-7.27253173790952,-0.291638083109205,
-0.319000042450751));
#12641=CARTESIAN_POINT('Ctrl Pts',(-7.57293190913717,-0.267199334594605,
-0.334700055185977));
#12642=CARTESIAN_POINT('Ctrl Pts',(-7.7182623784625,-0.00316037884059091,
-0.350400067921202));
#12643=CARTESIAN_POINT('Ctrl Pts',(-7.57820391972335,0.263712518683071,
-0.366100080656427));
#12644=CARTESIAN_POINT('Ctrl Pts',(-7.27834829656839,0.294111870889409,
-0.381800093391653));
#12645=CARTESIAN_POINT('Ctrl Pts',(-7.0875789229524,0.0607782868192583,
-0.397500106126878));
#12646=CARTESIAN_POINT('Ctrl Pts',(-7.17696052635036,-0.227055770079409,
-0.413200118862103));
#12647=CARTESIAN_POINT('Ctrl Pts',(-7.46634376553245,-0.311286739712534,
-0.428900131597328));
#12648=CARTESIAN_POINT('Ctrl Pts',(-7.69623591364813,-0.116383903440261,
-0.444600144332554));
#12649=CARTESIAN_POINT('Ctrl Pts',(-7.66049047611917,0.182881495483375,
-0.460300157067779));
#12650=CARTESIAN_POINT('Ctrl Pts',(-7.39116072945509,0.318155303117609,
-0.476000169803005));
#12651=CARTESIAN_POINT('Ctrl Pts',(-7.12975724182498,0.16813619780979,-0.49170018253823));
#12652=CARTESIAN_POINT('Ctrl Pts',(-7.11068302736388,-0.132652248309177,
-0.507400195273455));
#12653=CARTESIAN_POINT('Ctrl Pts',(-7.35104211921456,-0.31449015235472,
-0.523100208008681));
#12654=CARTESIAN_POINT('Ctrl Pts',(-7.63530220968826,-0.214321716488908,
-0.538800220743905));
#12655=CARTESIAN_POINT('Ctrl Pts',(-7.70856455690886,0.0780310521829601,
-0.554500233479132));
#12656=CARTESIAN_POINT('Ctrl Pts',(-7.50513409449975,0.300412640831581,
-0.570200246214356));
#12657=CARTESIAN_POINT('Ctrl Pts',(-7.20742890355809,0.253411306071293,
-0.585900258949583));
#12658=CARTESIAN_POINT('Ctrl Pts',(-7.08240401663227,-0.0208263248309716,
-0.601600271684806));
#12659=CARTESIAN_POINT('Ctrl Pts',(-7.24217058683982,-0.276388897598994,
-0.617300284420033));
#12660=CARTESIAN_POINT('Ctrl Pts',(-7.54346412051216,-0.28411067827933,
-0.633000297155257));
#12661=CARTESIAN_POINT('Ctrl Pts',(-7.71611237498659,-0.0370681238025536,
-0.648700309890484));
#12662=CARTESIAN_POINT('Ctrl Pts',(-7.60529887597468,0.243214651501716,
-0.664400322625709));
#12663=CARTESIAN_POINT('Ctrl Pts',(-7.31039342620376,0.305402743757612,
-0.680100335360934));
#12664=CARTESIAN_POINT('Ctrl Pts',(-7.09583598385675,0.0937368386372456,
-0.695800348096159));
#12665=CARTESIAN_POINT('Ctrl Pts',(-7.1540315175006,-0.201990993852965,
-0.711500360831385));
#12666=CARTESIAN_POINT('Ctrl Pts',(-7.43277687726091,-0.316577035174062,
-0.72720037356661));
#12667=CARTESIAN_POINT('Ctrl Pts',(-7.68215604714478,-0.147314711355987,
-0.742900386301836));
#12668=CARTESIAN_POINT('Ctrl Pts',(-7.67847246387183,0.1541052172216,-0.75860039903706));
#12669=CARTESIAN_POINT('Ctrl Pts',(-7.42518224851276,0.31721828408378,-0.774300411772287));
#12670=CARTESIAN_POINT('Ctrl Pts',(-7.14910431646667,0.1961203614586,-0.790000424507511));
#12671=CARTESIAN_POINT('Ctrl Pts',(-7.09842806627886,-0.10134084072585,
-0.805700437242737));
#12672=CARTESIAN_POINT('Ctrl Pts',(-7.24433403108591,-0.2381593775803,-0.816167112399554));
#12673=CARTESIAN_POINT('Ctrl Pts',(-7.3301933573839,-0.261113218593862,
-0.821400449977962));
#12674=CARTESIAN_POINT('Ctrl Pts',(-7.18048028959809,0.187686343907875,
0.0214004499779621));
#12675=CARTESIAN_POINT('Ctrl Pts',(-7.11876521010099,0.115503807360182,
0.0161671123995537));
#12676=CARTESIAN_POINT('Ctrl Pts',(-7.07309271989468,-0.0932943653013744,
0.00570043724273679));
#12677=CARTESIAN_POINT('Ctrl Pts',(-7.29776679845717,-0.324568420132722,
-0.00999957549248856));
#12678=CARTESIAN_POINT('Ctrl Pts',(-7.61418240376789,-0.264103422053756,
-0.0256995882277139));
#12679=CARTESIAN_POINT('Ctrl Pts',(-7.73850299036808,0.0328477914664162,
-0.0413996009629393));
#12680=CARTESIAN_POINT('Ctrl Pts',(-7.55930261173826,0.300510993938772,
-0.0570996136981645));
#12681=CARTESIAN_POINT('Ctrl Pts',(-7.23724515539316,0.298620370859126,
-0.0727996264333899));
#12682=CARTESIAN_POINT('Ctrl Pts',(-7.06113594291133,0.0289950208638007,
-0.0884996391686152));
#12683=CARTESIAN_POINT('Ctrl Pts',(-7.18888719273634,-0.26665078603973,
-0.104199651903841));
#12684=CARTESIAN_POINT('Ctrl Pts',(-7.50594640747463,-0.323178186775197,
-0.119899664639066));
#12685=CARTESIAN_POINT('Ctrl Pts',(-7.72800192402634,-0.0899136096583525,
-0.135599677374291));
#12686=CARTESIAN_POINT('Ctrl Pts',(-7.65593523548524,0.223979844613395,
-0.151299690109517));
#12687=CARTESIAN_POINT('Ctrl Pts',(-7.35436883360446,0.337027193253441,
-0.166999702844742));
#12688=CARTESIAN_POINT('Ctrl Pts',(-7.09372040202686,0.147859634458496,
-0.182699715579967));
#12689=CARTESIAN_POINT('Ctrl Pts',(-7.10771579171938,-0.173895379574711,
-0.198399728315193));
#12690=CARTESIAN_POINT('Ctrl Pts',(-7.3838052511641,-0.339716588449989,
-0.214099741050418));
#12691=CARTESIAN_POINT('Ctrl Pts',(-7.67441668925201,-0.200910747760891,
-0.229799753785643));
#12692=CARTESIAN_POINT('Ctrl Pts',(-7.71895605342194,0.11805372478634,-0.245499766520869));
#12693=CARTESIAN_POINT('Ctrl Pts',(-7.47748446259449,0.331158271467761,
-0.261199779256094));
#12694=CARTESIAN_POINT('Ctrl Pts',(-7.16653181178222,0.247310028207208,
-0.276899791991319));
#12695=CARTESIAN_POINT('Ctrl Pts',(-7.06493232465333,-0.0583034944304196,
-0.292599804726545));
#12696=CARTESIAN_POINT('Ctrl Pts',(-7.26379123674133,-0.311635712042882,
-0.30829981746177));
#12697=CARTESIAN_POINT('Ctrl Pts',(-7.58478985345242,-0.285521198075471,
-0.323999830196996));
#12698=CARTESIAN_POINT('Ctrl Pts',(-7.7400856358375,-0.00337708607810321,
-0.339699842932221));
#12699=CARTESIAN_POINT('Ctrl Pts',(-7.59042336590528,0.28179529113023,-0.355399855667446));
#12700=CARTESIAN_POINT('Ctrl Pts',(-7.27000663693862,0.314279127498463,
-0.371099868402672));
#12701=CARTESIAN_POINT('Ctrl Pts',(-7.06615620372709,0.0649458551082769,
-0.386799881137897));
#12702=CARTESIAN_POINT('Ctrl Pts',(-7.16166670537864,-0.242624988574094,
-0.402499893873122));
#12703=CARTESIAN_POINT('Ctrl Pts',(-7.47089295880322,-0.332631677405099,
-0.418199906608348));
#12704=CARTESIAN_POINT('Ctrl Pts',(-7.71654881590975,-0.124364349923924,
-0.433899919343572));
#12705=CARTESIAN_POINT('Ctrl Pts',(-7.67835231304613,0.195421683124586,
-0.449599932078799));
#12706=CARTESIAN_POINT('Ctrl Pts',(-7.39055462050486,0.339971218334158,
-0.465299944814023));
#12707=CARTESIAN_POINT('Ctrl Pts',(-7.11122669073103,0.179665300107655,
-0.48099995754925));
#12708=CARTESIAN_POINT('Ctrl Pts',(-7.09084455701971,-0.141748215511483,
-0.496699970284474));
#12709=CARTESIAN_POINT('Ctrl Pts',(-7.34768507639324,-0.336054748113396,
-0.512399983019701));
#12710=CARTESIAN_POINT('Ctrl Pts',(-7.65143688670457,-0.229017760685471,
-0.528099995754924));
#12711=CARTESIAN_POINT('Ctrl Pts',(-7.72972283447454,0.083381642922767,
-0.543800008490151));
#12712=CARTESIAN_POINT('Ctrl Pts',(-7.51234314136931,0.321011941356013,
-0.559500021225375));
#12713=CARTESIAN_POINT('Ctrl Pts',(-7.19422429979393,0.270787724172747,
-0.575200033960601));
#12714=CARTESIAN_POINT('Ctrl Pts',(-7.06062645398167,-0.0222543863227421,
-0.590900046695826));
#12715=CARTESIAN_POINT('Ctrl Pts',(-7.23134822096239,-0.295340889590735,
-0.606600059431052));
#12716=CARTESIAN_POINT('Ctrl Pts',(-7.55330145799812,-0.303592152919931,
-0.622300072166277));
#12717=CARTESIAN_POINT('Ctrl Pts',(-7.73778820658214,-0.0396098857602792,
-0.638000084901502));
#12718=CARTESIAN_POINT('Ctrl Pts',(-7.6193762238247,0.259891884804417,-0.653700097636727));
#12719=CARTESIAN_POINT('Ctrl Pts',(-7.30424910172566,0.326344215735072,
-0.669400110371953));
#12720=CARTESIAN_POINT('Ctrl Pts',(-7.07497945145549,0.100164375454451,
-0.685100123107178));
#12721=CARTESIAN_POINT('Ctrl Pts',(-7.13716545395374,-0.215841520162671,
-0.700800135842404));
#12722=CARTESIAN_POINT('Ctrl Pts',(-7.43502438836124,-0.338284728527552,
-0.716500148577629));
#12723=CARTESIAN_POINT('Ctrl Pts',(-7.70150349269112,-0.157416083929697,
-0.732200161312854));
#12724=CARTESIAN_POINT('Ctrl Pts',(-7.69756732604273,0.164672214912321,
-0.74790017404808));
#12725=CARTESIAN_POINT('Ctrl Pts',(-7.42690899577466,0.338969947887268,
-0.763600186783304));
#12726=CARTESIAN_POINT('Ctrl Pts',(-7.13190039465073,0.209568338392803,
-0.779300199518531));
#12727=CARTESIAN_POINT('Ctrl Pts',(-7.07774927301882,-0.108289784111627,
-0.795000212253755));
#12728=CARTESIAN_POINT('Ctrl Pts',(-7.2336600126218,-0.254489970653575,
-0.805466887410573));
#12729=CARTESIAN_POINT('Ctrl Pts',(-7.32540671456531,-0.279017756984216,
-0.810700224988981));
#12730=CARTESIAN_POINT('Ctrl Pts',(-7.16639373423038,0.199730155693065,
0.0321006749669432));
#12731=CARTESIAN_POINT('Ctrl Pts',(-7.10071840495542,0.122915673814364,
0.0268673373885347));
#12732=CARTESIAN_POINT('Ctrl Pts',(-7.05211511613929,-0.0992810543321975,
0.0164006622317178));
#12733=CARTESIAN_POINT('Ctrl Pts',(-7.29120650530028,-0.345395939504156,
0.000700649496492501));
#12734=CARTESIAN_POINT('Ctrl Pts',(-7.62792646476333,-0.281050909232692,
-0.0149993632387328));
#12735=CARTESIAN_POINT('Ctrl Pts',(-7.76022468955957,0.0349556305864266,
-0.0306993759739582));
#12736=CARTESIAN_POINT('Ctrl Pts',(-7.56952504259133,0.319794750950713,
-0.0463993887091835));
#12737=CARTESIAN_POINT('Ctrl Pts',(-7.2268011951414,0.317782806798611,-0.0620994014444089));
#12738=CARTESIAN_POINT('Ctrl Pts',(-7.03939107410859,0.0308556281233394,
-0.0777994141796342));
#12739=CARTESIAN_POINT('Ctrl Pts',(-7.17534010740672,-0.283761737281935,
-0.0934994269148595));
#12740=CARTESIAN_POINT('Ctrl Pts',(-7.51274497664259,-0.343916495026914,
-0.109199439650085));
#12741=CARTESIAN_POINT('Ctrl Pts',(-7.74904977096025,-0.0956833559760907,
-0.12489945238531));
#12742=CARTESIAN_POINT('Ctrl Pts',(-7.67235857104177,0.238352606296705,
-0.140599465120536));
#12743=CARTESIAN_POINT('Ctrl Pts',(-7.351440686739,0.358654190708449,-0.156299477855761));
#12744=CARTESIAN_POINT('Ctrl Pts',(-7.07406647433649,0.15734777073398,-0.171999490590986));
#12745=CARTESIAN_POINT('Ctrl Pts',(-7.08895994662689,-0.185054226714597,
-0.187699503326211));
#12746=CARTESIAN_POINT('Ctrl Pts',(-7.38276603593497,-0.36151616409523,
-0.203399516061437));
#12747=CARTESIAN_POINT('Ctrl Pts',(-7.69202597763844,-0.213803168068474,
-0.219099528796662));
#12748=CARTESIAN_POINT('Ctrl Pts',(-7.73942342784661,0.125629219157764,
-0.234799541531888));
#12749=CARTESIAN_POINT('Ctrl Pts',(-7.48245663192943,0.352408660865427,
-0.250499554267113));
#12750=CARTESIAN_POINT('Ctrl Pts',(-7.15155018414657,0.263179885173358,
-0.266199567002338));
#12751=CARTESIAN_POINT('Ctrl Pts',(-7.04343106924415,-0.0620448231745263,
-0.281899579737564));
#12752=CARTESIAN_POINT('Ctrl Pts',(-7.25505073557315,-0.331633340976559,
-0.297599592472789));
#12753=CARTESIAN_POINT('Ctrl Pts',(-7.59664779776768,-0.303843061556337,
-0.313299605208015));
#12754=CARTESIAN_POINT('Ctrl Pts',(-7.76190889321249,-0.00359379331561558,
-0.328999617943239));
#12755=CARTESIAN_POINT('Ctrl Pts',(-7.60264281208722,0.299878063577389,
-0.344699630678465));
#12756=CARTESIAN_POINT('Ctrl Pts',(-7.26166497730884,0.334446384107517,
-0.36039964341369));
#12757=CARTESIAN_POINT('Ctrl Pts',(-7.04473348450178,0.0691134233972956,
-0.376099656148916));
#12758=CARTESIAN_POINT('Ctrl Pts',(-7.14637288440692,-0.258194207068779,
-0.391799668884141));
#12759=CARTESIAN_POINT('Ctrl Pts',(-7.47544215207399,-0.353976615097665,
-0.407499681619366));
#12760=CARTESIAN_POINT('Ctrl Pts',(-7.73686171817138,-0.132344796407588,
-0.423199694354592));
#12761=CARTESIAN_POINT('Ctrl Pts',(-7.69621414997308,0.207961870765797,
-0.438899707089817));
#12762=CARTESIAN_POINT('Ctrl Pts',(-7.38994851155463,0.361787133550707,
-0.454599719825042));
#12763=CARTESIAN_POINT('Ctrl Pts',(-7.09269613963708,0.191194402405521,
-0.470299732560268));
#12764=CARTESIAN_POINT('Ctrl Pts',(-7.07100608667554,-0.15084418271379,
-0.485999745295493));
#12765=CARTESIAN_POINT('Ctrl Pts',(-7.34432803357192,-0.357619343872072,
-0.501699758030719));
#12766=CARTESIAN_POINT('Ctrl Pts',(-7.66757156372086,-0.243713804882034,
-0.517399770765943));
#12767=CARTESIAN_POINT('Ctrl Pts',(-7.75088111204022,0.0887322336625739,
-0.53309978350117));
#12768=CARTESIAN_POINT('Ctrl Pts',(-7.51955218823887,0.341611241880446,
-0.548799796236394));
#12769=CARTESIAN_POINT('Ctrl Pts',(-7.18101969602976,0.288164142274201,
-0.56449980897162));
#12770=CARTESIAN_POINT('Ctrl Pts',(-7.03884889133106,-0.0236824478145123,
-0.580199821706845));
#12771=CARTESIAN_POINT('Ctrl Pts',(-7.22052585508497,-0.314292881582478,
-0.595899834442071));
#12772=CARTESIAN_POINT('Ctrl Pts',(-7.56313879548406,-0.323073627560531,
-0.611599847177296));
#12773=CARTESIAN_POINT('Ctrl Pts',(-7.75946403817769,-0.0421516477180053,
-0.627299859912521));
#12774=CARTESIAN_POINT('Ctrl Pts',(-7.63345357167473,0.276569118107119,
-0.642999872647746));
#12775=CARTESIAN_POINT('Ctrl Pts',(-7.29810477724755,0.347285687712531,
-0.658699885382972));
#12776=CARTESIAN_POINT('Ctrl Pts',(-7.05412291905423,0.106591912271656,
-0.674399898118197));
#12777=CARTESIAN_POINT('Ctrl Pts',(-7.12029939040689,-0.229692046472377,
-0.690099910853423));
#12778=CARTESIAN_POINT('Ctrl Pts',(-7.43727189946158,-0.359992421881043,
-0.705799923588648));
#12779=CARTESIAN_POINT('Ctrl Pts',(-7.72085093823746,-0.167517456503407,
-0.721499936323873));
#12780=CARTESIAN_POINT('Ctrl Pts',(-7.71666218821363,0.175239212603042,
-0.737199949059098));
#12781=CARTESIAN_POINT('Ctrl Pts',(-7.42863574303655,0.360721611690756,
-0.752899961794324));
#12782=CARTESIAN_POINT('Ctrl Pts',(-7.1146964728348,0.223016315327006,-0.768599974529548));
#12783=CARTESIAN_POINT('Ctrl Pts',(-7.05707047975879,-0.115238727497404,
-0.784299987264776));
#12784=CARTESIAN_POINT('Ctrl Pts',(-7.22298599415769,-0.270820563726849,
-0.794766662421592));
#12785=CARTESIAN_POINT('Ctrl Pts',(-7.32062007174671,-0.29692229537457,
-0.8));
#12786=CARTESIAN_POINT('Ctrl Pts',(-7.20865340033349,0.163598720337495,
0.));
#12787=CARTESIAN_POINT('Ctrl Pts',(-7.19749016426694,0.153108019593971,
-2.76372499376297E-18));
#12788=CARTESIAN_POINT('Ctrl Pts',(-7.18742993143982,0.141586713971671,
-8.45132788489384E-17));
#12789=CARTESIAN_POINT('Ctrl Pts',(-7.1784776381451,0.129252304447995,-5.46437894932694E-17));
#12790=CARTESIAN_POINT('Ctrl Pts',(-7.17047115113201,0.118221020461395,
-2.79299999936894E-17));
#12791=CARTESIAN_POINT('Ctrl Pts',(-7.16335084130231,0.106538037408676,
2.44997822749073E-17));
#12792=CARTESIAN_POINT('Ctrl Pts',(-7.15713966083231,0.0943314427665496,
2.60208521396521E-17));
#12793=CARTESIAN_POINT('Ctrl Pts',(-7.15505924455693,0.0902428804903266,
2.65303299302091E-17));
#12794=CARTESIAN_POINT('Ctrl Pts',(-7.15308034324392,0.0860939263230946,
-2.27985261165535E-17));
#12795=CARTESIAN_POINT('Ctrl Pts',(-7.15120644281776,0.0818935847012138,
-2.16840434497101E-17));
#12796=CARTESIAN_POINT('Ctrl Pts',(-7.14450619729809,0.0668750064778017,
-1.76991425494042E-17));
#12797=CARTESIAN_POINT('Ctrl Pts',(-7.13918883905698,0.0513023322829503,
3.17673853203519E-17));
#12798=CARTESIAN_POINT('Ctrl Pts',(-7.13527708034929,0.0354016414449469,
2.94902990916057E-17));
#12799=CARTESIAN_POINT('Ctrl Pts',(-7.13257231819721,0.0244072039082036,
2.79158214438866E-17));
#12800=CARTESIAN_POINT('Ctrl Pts',(-7.13054023888487,0.0132548753996132,
-1.66159572056239E-18));
#12801=CARTESIAN_POINT('Ctrl Pts',(-7.12920017560294,0.00201107170221857,
-5.20417042793042E-18));
#12802=CARTESIAN_POINT('Ctrl Pts',(-7.12844522682347,-0.00432332757017003,
-7.1999436780392E-18));
#12803=CARTESIAN_POINT('Ctrl Pts',(-7.1279101003675,-0.0106868532653293,
2.05898758024937E-17));
#12804=CARTESIAN_POINT('Ctrl Pts',(-7.12759984712261,-0.0170680571507328,
1.90819582357449E-17));
#12805=CARTESIAN_POINT('Ctrl Pts',(-7.12738957317498,-0.021392914194958,
1.80599680239007E-17));
#12806=CARTESIAN_POINT('Ctrl Pts',(-7.12728309197496,-0.0257168244094562,
-4.90358507150565E-18));
#12807=CARTESIAN_POINT('Ctrl Pts',(-7.12728089724359,-0.0300343251795264,
-5.20417042793042E-18));
#12808=CARTESIAN_POINT('Ctrl Pts',(-7.12727288296517,-0.0458001057272751,
-6.30178754895358E-18));
#12809=CARTESIAN_POINT('Ctrl Pts',(-7.12865222250825,-0.0614865713174629,
6.0937287207194E-17));
#12810=CARTESIAN_POINT('Ctrl Pts',(-7.13146167838013,-0.0769179188083685,
6.93889390390723E-17));
#12811=CARTESIAN_POINT('Ctrl Pts',(-7.13378015998439,-0.0896525182889436,
7.27129920200424E-17));
#12812=CARTESIAN_POINT('Ctrl Pts',(-7.13707306322478,-0.102214075074238,
5.18772623636705E-17));
#12813=CARTESIAN_POINT('Ctrl Pts',(-7.1412671846214,-0.114535293399235,
3.12250225675825E-17));
#12814=CARTESIAN_POINT('Ctrl Pts',(-7.14321202162556,-0.120248709647508,
2.16484661506902E-17));
#12815=CARTESIAN_POINT('Ctrl Pts',(-7.14535294266045,-0.125914390083585,
4.01380311714632E-17));
#12816=CARTESIAN_POINT('Ctrl Pts',(-7.14767192915255,-0.131498838079198,
3.81639164714898E-17));
#12817=CARTESIAN_POINT('Ctrl Pts',(-7.15418636647591,-0.14718652603121,
3.26182841334338E-17));
#12818=CARTESIAN_POINT('Ctrl Pts',(-7.16211292622978,-0.162272159028203,
2.16855313984206E-17));
#12819=CARTESIAN_POINT('Ctrl Pts',(-7.17127396198873,-0.176613249443012,
-1.04083408558608E-17));
#12820=CARTESIAN_POINT('Ctrl Pts',(-7.17662531782903,-0.18499049847543,
-2.91557549305296E-17));
#12821=CARTESIAN_POINT('Ctrl Pts',(-7.18239894289445,-0.193113697063826,
2.13680762433296E-17));
#12822=CARTESIAN_POINT('Ctrl Pts',(-7.18856704204723,-0.200952684844035,
2.08166817117217E-17));
#12823=CARTESIAN_POINT('Ctrl Pts',(-7.19257962089004,-0.206052239137303,
2.04579789774165E-17));
#12824=CARTESIAN_POINT('Ctrl Pts',(-7.1967592496289,-0.211031481079785,
3.56529973313533E-17));
#12825=CARTESIAN_POINT('Ctrl Pts',(-7.20109934731034,-0.215881483781976,
3.81639164714898E-17));
#12826=CARTESIAN_POINT('Ctrl Pts',(-7.20432878913168,-0.219490343008123,
4.00322770191852E-17));
#12827=CARTESIAN_POINT('Ctrl Pts',(-7.20764437108191,-0.223024398793103,
4.33361061948454E-19));
#12828=CARTESIAN_POINT('Ctrl Pts',(-7.21103723976682,-0.226474616868443,
3.46944695195361E-18));
#12829=CARTESIAN_POINT('Ctrl Pts',(-7.22024722842187,-0.235840281231676,
1.17109438089107E-17));
#12830=CARTESIAN_POINT('Ctrl Pts',(-7.23003736548959,-0.24460178169824,
3.42136972519736E-17));
#12831=CARTESIAN_POINT('Ctrl Pts',(-7.24034429477035,-0.252691942380673,
3.12250225675825E-17));
#12832=CARTESIAN_POINT('Ctrl Pts',(-7.24508022119563,-0.256409286772693,
2.98517577445839E-17));
#12833=CARTESIAN_POINT('Ctrl Pts',(-7.24992543835673,-0.259984791203115,
2.74594575473033E-17));
#12834=CARTESIAN_POINT('Ctrl Pts',(-7.25487463133442,-0.263411298803592,
1.73472347597681E-17));
#12835=CARTESIAN_POINT('Ctrl Pts',(-7.26003204798081,-0.266981967277684,
6.80956803886786E-18));
#12836=CARTESIAN_POINT('Ctrl Pts',(-7.26529590651007,-0.270386211806602,
-2.31583854274773E-17));
#12837=CARTESIAN_POINT('Ctrl Pts',(-7.27065460638826,-0.273613872126434,
-2.08166817117217E-17));
#12838=CARTESIAN_POINT('Ctrl Pts',(-7.28259601671275,-0.280806440686599,
-1.55983926558145E-17));
#12839=CARTESIAN_POINT('Ctrl Pts',(-7.29501481903722,-0.287128105902613,
9.97222803653275E-18));
#12840=CARTESIAN_POINT('Ctrl Pts',(-7.30784325376688,-0.292493143353308,
-6.93889390390723E-18));
#12841=CARTESIAN_POINT('Ctrl Pts',(-7.31199336468935,-0.29422877992884,
-1.2253478561421E-17));
#12842=CARTESIAN_POINT('Ctrl Pts',(-7.31618644117717,-0.295864187143585,
2.68855459144816E-18));
#12843=CARTESIAN_POINT('Ctrl Pts',(-7.32041913648099,-0.297400286396329,
0.));
#12844=CARTESIAN_POINT('Ctrl Pts',(-7.65166448275063,-0.000213511554003356,
-0.161258330249198));
#12845=CARTESIAN_POINT('Ctrl Pts',(-7.65185372337913,-0.0226803085523069,
-0.15983892928355));
#12846=CARTESIAN_POINT('Ctrl Pts',(-7.64908704070277,-0.0451012973586514,
-0.158419528317902));
#12847=CARTESIAN_POINT('Ctrl Pts',(-7.64317712569085,-0.0666606195194149,
-0.157000127352254));
#12848=CARTESIAN_POINT('Ctrl Pts',(-7.62138724315195,-0.146149934772504,
-0.151766789773845));
#12849=CARTESIAN_POINT('Ctrl Pts',(-7.55686825614531,-0.213925752522132,
-0.146533452195437));
#12850=CARTESIAN_POINT('Ctrl Pts',(-7.47854744501815,-0.239601546944206,
-0.141300114617028));
#12851=CARTESIAN_POINT('Ctrl Pts',(-7.40022663389099,-0.265277341366279,
-0.13606677703862));
#12852=CARTESIAN_POINT('Ctrl Pts',(-7.3081039986433,-0.248853112460798,
-0.130833439460212));
#12853=CARTESIAN_POINT('Ctrl Pts',(-7.24348340053965,-0.197690549691385,
-0.125600101881803));
#12854=CARTESIAN_POINT('Ctrl Pts',(-7.17886280243601,-0.146527986921971,
-0.120366764303395));
#12855=CARTESIAN_POINT('Ctrl Pts',(-7.14174424147641,-0.0606270902886238,
-0.115133426724986));
#12856=CARTESIAN_POINT('Ctrl Pts',(-7.14876952689325,0.0214936401339547,
-0.109900089146578));
#12857=CARTESIAN_POINT('Ctrl Pts',(-7.1557948123101,0.103614370556533,-0.104666751568169));
#12858=CARTESIAN_POINT('Ctrl Pts',(-7.20696394410339,0.181954934768343,
-0.099433413989761));
#12859=CARTESIAN_POINT('Ctrl Pts',(-7.27933595568927,0.221399880363371,
-0.0942000764113526));
#12860=CARTESIAN_POINT('Ctrl Pts',(-7.35170796727516,0.260844825958399,
-0.0889667388329441));
#12861=CARTESIAN_POINT('Ctrl Pts',(-7.44528285865364,0.261394152936645,
-0.0837334012545357));
#12862=CARTESIAN_POINT('Ctrl Pts',(-7.51810394466837,0.222783588644352,
-0.0785000636761272));
#12863=CARTESIAN_POINT('Ctrl Pts',(-7.59092503068311,0.184173024352059,
-0.0732667260977187));
#12864=CARTESIAN_POINT('Ctrl Pts',(-7.64299231133411,0.106402568789228,
-0.0680333885193103));
#12865=CARTESIAN_POINT('Ctrl Pts',(-7.65096506662493,0.0243772475207652,
-0.0628000509409019));
#12866=CARTESIAN_POINT('Ctrl Pts',(-7.6517479807543,0.0163224683829433,
-0.0622861440436673));
#12867=CARTESIAN_POINT('Ctrl Pts',(-7.6521056921332,0.00822665964822356,
-0.0617722371464327));
#12868=CARTESIAN_POINT('Ctrl Pts',(-7.65205352925247,0.000126382978640343,
-0.0612583302491982));
#12869=CARTESIAN_POINT('Ctrl Pts',(-7.47937992825329,-0.29692229537457,
0.));
#12870=CARTESIAN_POINT('Ctrl Pts',(-7.57701400584231,-0.270820563726849,
-0.00523333757840845));
#12871=CARTESIAN_POINT('Ctrl Pts',(-7.74292936377346,-0.115237711690175,
-0.0157000127352254));
#12872=CARTESIAN_POINT('Ctrl Pts',(-7.68530366248674,0.2230159413608,-0.0314000254704506));
#12873=CARTESIAN_POINT('Ctrl Pts',(-7.37136424514298,0.36072194419717,-0.0471000382056761));
#12874=CARTESIAN_POINT('Ctrl Pts',(-7.0833377209053,0.175239119455976,-0.0628000509409012));
#12875=CARTESIAN_POINT('Ctrl Pts',(-7.07914899542098,-0.167517421922754,
-0.0785000636761269));
#12876=CARTESIAN_POINT('Ctrl Pts',(-7.3627280810489,-0.359992553262469,
-0.0942000764113519));
#12877=CARTESIAN_POINT('Ctrl Pts',(-7.67970068592657,-0.229692080624575,
-0.109900089146577));
#12878=CARTESIAN_POINT('Ctrl Pts',(-7.74587716255528,0.106591926360324,
-0.125600101881803));
#12879=CARTESIAN_POINT('Ctrl Pts',(-7.50189525062872,0.347285780617978,
-0.141300114617028));
#12880=CARTESIAN_POINT('Ctrl Pts',(-7.16654636885183,0.276569183243976,
-0.157000127352254));
#12881=CARTESIAN_POINT('Ctrl Pts',(-7.04053587339322,-0.0421516562996225,
-0.172700140087479));
#12882=CARTESIAN_POINT('Ctrl Pts',(-7.23686116352416,-0.323073708797981,
-0.188400152822704));
#12883=CARTESIAN_POINT('Ctrl Pts',(-7.5794741897514,-0.314292959115147,
-0.204100165557929));
#12884=CARTESIAN_POINT('Ctrl Pts',(-7.76115119822227,-0.0236824539723921,
-0.219800178293155));
#12885=CARTESIAN_POINT('Ctrl Pts',(-7.61898035843412,0.288164213987784,
-0.23550019102838));
#12886=CARTESIAN_POINT('Ctrl Pts',(-7.28044778202723,0.341611326648396,
-0.251200203763605));
#12887=CARTESIAN_POINT('Ctrl Pts',(-7.04911880083639,0.0887322557395692,
-0.266900216498831));
#12888=CARTESIAN_POINT('Ctrl Pts',(-7.13242836981262,-0.243713865431744,
-0.282600229234056));
#12889=CARTESIAN_POINT('Ctrl Pts',(-7.45567198026117,-0.357619432680664,
-0.298300241969282));
#12890=CARTESIAN_POINT('Ctrl Pts',(-7.72899399503084,-0.150844220183267,
-0.314000254704507));
#12891=CARTESIAN_POINT('Ctrl Pts',(-7.70730393668735,0.191194449893827,
-0.329700267439732));
#12892=CARTESIAN_POINT('Ctrl Pts',(-7.41005149094087,0.36178722340353,-0.345400280174957));
#12893=CARTESIAN_POINT('Ctrl Pts',(-7.10378577645897,0.207961922416443,
-0.361100292910183));
#12894=CARTESIAN_POINT('Ctrl Pts',(-7.06313819816462,-0.132344829277446,
-0.376800305645408));
#12895=CARTESIAN_POINT('Ctrl Pts',(-7.32455782918916,-0.35397670301188,
-0.392500318380633));
#12896=CARTESIAN_POINT('Ctrl Pts',(-7.65362717858442,-0.25819427119465,
-0.408200331115859));
#12897=CARTESIAN_POINT('Ctrl Pts',(-7.75526660373307,0.069113440562637,
-0.423900343851084));
#12898=CARTESIAN_POINT('Ctrl Pts',(-7.53833505704833,0.334446467171126,
-0.43960035658631));
#12899=CARTESIAN_POINT('Ctrl Pts',(-7.19735713758398,0.299878138056265,
-0.455300369321535));
#12900=CARTESIAN_POINT('Ctrl Pts',(-7.03809101690294,-0.0035937942090703,
-0.47100038205676));
#12901=CARTESIAN_POINT('Ctrl Pts',(-7.20335215339251,-0.30384313701778,
-0.486700394791986));
#12902=CARTESIAN_POINT('Ctrl Pts',(-7.54494930042661,-0.331633423345088,
-0.50240040752721));
#12903=CARTESIAN_POINT('Ctrl Pts',(-7.75656901931451,-0.0620448385777456,
-0.518100420262437));
#12904=CARTESIAN_POINT('Ctrl Pts',(-7.64844987755816,0.263179950525062,
-0.533800432997661));
#12905=CARTESIAN_POINT('Ctrl Pts',(-7.31754334759326,0.352408748413955,
-0.549500445732887));
#12906=CARTESIAN_POINT('Ctrl Pts',(-7.06057648784951,0.125629250314373,
-0.565200458468112));
#12907=CARTESIAN_POINT('Ctrl Pts',(-7.10797394984171,-0.213803221083396,
-0.580900471203338));
#12908=CARTESIAN_POINT('Ctrl Pts',(-7.41723396832727,-0.361516254045136,
-0.596600483938562));
#12909=CARTESIAN_POINT('Ctrl Pts',(-7.71104013066228,-0.185054272366607,
-0.612300496673789));
#12910=CARTESIAN_POINT('Ctrl Pts',(-7.72593360653096,0.157347809231622,
-0.628000509409013));
#12911=CARTESIAN_POINT('Ctrl Pts',(-7.44855932549587,0.358654280875835,
-0.643700522144239));
#12912=CARTESIAN_POINT('Ctrl Pts',(-7.12764136094462,0.238352663458736,
-0.659400534879464));
#12913=CARTESIAN_POINT('Ctrl Pts',(-7.05095014313138,-0.0956833759672795,
-0.675100547614689));
#12914=CARTESIAN_POINT('Ctrl Pts',(-7.28725499370478,-0.34391658738075,
-0.690800560349915));
#12915=CARTESIAN_POINT('Ctrl Pts',(-7.62465995186745,-0.283761795119453,
-0.70650057308514));
#12916=CARTESIAN_POINT('Ctrl Pts',(-7.76060900814316,0.0308556130297948,
-0.722200585820366));
#12917=CARTESIAN_POINT('Ctrl Pts',(-7.57319886321716,0.317782926109968,
-0.737900598555591));
#12918=CARTESIAN_POINT('Ctrl Pts',(-7.23047488314852,0.319794760031351,
-0.753600611290816));
#12919=CARTESIAN_POINT('Ctrl Pts',(-7.03977528830754,0.0349557588279105,
-0.769300624026042));
#12920=CARTESIAN_POINT('Ctrl Pts',(-7.17207333714996,-0.281051176556267,
-0.785000636761267));
#12921=CARTESIAN_POINT('Ctrl Pts',(-7.50879381804844,-0.345395707969619,
-0.800700649496492));
#12922=CARTESIAN_POINT('Ctrl Pts',(-7.74788417951995,-0.0992818028310835,
-0.816400662231718));
#12923=CARTESIAN_POINT('Ctrl Pts',(-7.69928159504458,0.122915673814362,
-0.826867337388535));
#12924=CARTESIAN_POINT('Ctrl Pts',(-7.63360626576962,0.199730155693063,
-0.832100674966943));
#12925=CARTESIAN_POINT('Ctrl Pts',(-7.47459328543469,-0.279017756984216,
0.0107002249889811));
#12926=CARTESIAN_POINT('Ctrl Pts',(-7.5663399873782,-0.254489970653575,
0.00546688741057261));
#12927=CARTESIAN_POINT('Ctrl Pts',(-7.7222505799485,-0.108288829557998,
-0.0049997877462443));
#12928=CARTESIAN_POINT('Ctrl Pts',(-7.66809973251085,0.209567986976916,
-0.0206998004814696));
#12929=CARTESIAN_POINT('Ctrl Pts',(-7.37309099311766,0.338970260343406,
-0.036399813216695));
#12930=CARTESIAN_POINT('Ctrl Pts',(-7.10243258855636,0.164672127382063,
-0.0520998259519203));
#12931=CARTESIAN_POINT('Ctrl Pts',(-7.09849644496774,-0.157416051434272,
-0.0677998386871457));
#12932=CARTESIAN_POINT('Ctrl Pts',(-7.36497559332446,-0.338284851986623,
-0.083499851422371));
#12933=CARTESIAN_POINT('Ctrl Pts',(-7.66283461777677,-0.215841552255477,
-0.0991998641575963));
#12934=CARTESIAN_POINT('Ctrl Pts',(-7.72502062523293,0.100164388693566,
-0.114899876892822));
#12935=CARTESIAN_POINT('Ctrl Pts',(-7.49575092446967,0.326344303038281,
-0.130599889628047));
#12936=CARTESIAN_POINT('Ctrl Pts',(-7.18062372028813,0.259891946013495,
-0.146299902363272));
#12937=CARTESIAN_POINT('Ctrl Pts',(-7.06221171032109,-0.0396098938244216,
-0.161999915098498));
#12938=CARTESIAN_POINT('Ctrl Pts',(-7.24669850348192,-0.303592229258729,
-0.177699927833723));
#12939=CARTESIAN_POINT('Ctrl Pts',(-7.56865182117034,-0.295340962448153,
-0.193399940568948));
#12940=CARTESIAN_POINT('Ctrl Pts',(-7.73937363017156,-0.022254392109299,
-0.209099953304174));
#12941=CARTESIAN_POINT('Ctrl Pts',(-7.60577575138577,0.270787791561971,
-0.224799966039399));
#12942=CARTESIAN_POINT('Ctrl Pts',(-7.28765683068976,0.321012021012421,
-0.240499978774624));
#12943=CARTESIAN_POINT('Ctrl Pts',(-7.07027708365565,0.0833816636685102,
-0.25619999150985));
#12944=CARTESIAN_POINT('Ctrl Pts',(-7.14856305083687,-0.229017817584008,
-0.271900004245075));
#12945=CARTESIAN_POINT('Ctrl Pts',(-7.4523149366057,-0.336054831566793,
-0.287600016980301));
#12946=CARTESIAN_POINT('Ctrl Pts',(-7.70915551975974,-0.141748250721535,
-0.303300029715525));
#12947=CARTESIAN_POINT('Ctrl Pts',(-7.688773380991,0.179665344732397,-0.319000042450751));
#12948=CARTESIAN_POINT('Ctrl Pts',(-7.40944538184016,0.339971302768818,
-0.334700055185976));
#12949=CARTESIAN_POINT('Ctrl Pts',(-7.12164761782211,0.195421731660677,
-0.350400067921202));
#12950=CARTESIAN_POINT('Ctrl Pts',(-7.08345110547122,-0.124364380811717,
-0.366100080656427));
#12951=CARTESIAN_POINT('Ctrl Pts',(-7.32910702358977,-0.33263176001805,
-0.381800093391652));
#12952=CARTESIAN_POINT('Ctrl Pts',(-7.6383333538143,-0.242625048833148,
-0.397500106126878));
#12953=CARTESIAN_POINT('Ctrl Pts',(-7.73384387918716,0.064945871238541,
-0.413200118862103));
#12954=CARTESIAN_POINT('Ctrl Pts',(-7.52999339534681,0.314279205553302,
-0.428900131597329));
#12955=CARTESIAN_POINT('Ctrl Pts',(-7.20957658680075,0.281795361117998,
-0.444600144332554));
#12956=CARTESIAN_POINT('Ctrl Pts',(-7.05991427969802,-0.00337708691768223,
-0.460300157067779));
#12957=CARTESIAN_POINT('Ctrl Pts',(-7.21521010065283,-0.285521268986558,
-0.476000169803004));
#12958=CARTESIAN_POINT('Ctrl Pts',(-7.53620879708761,-0.311635789444555,
-0.49170018253823));
#12959=CARTESIAN_POINT('Ctrl Pts',(-7.73506775856522,-0.0583035089048183,
-0.507400195273455));
#12960=CARTESIAN_POINT('Ctrl Pts',(-7.63346824620169,0.247310089618177,
-0.523100208008681));
#12961=CARTESIAN_POINT('Ctrl Pts',(-7.32251551816297,0.331158353737076,
-0.538800220743905));
#12962=CARTESIAN_POINT('Ctrl Pts',(-7.08104386735775,0.118053754064193,
-0.554500233479132));
#12963=CARTESIAN_POINT('Ctrl Pts',(-7.12558324260111,-0.200910797578991,
-0.570200246214356));
#12964=CARTESIAN_POINT('Ctrl Pts',(-7.41619475284112,-0.339716672975878,
-0.585900258949582));
#12965=CARTESIAN_POINT('Ctrl Pts',(-7.6922842809092,-0.173895422473886,
-0.601600271684807));
#12966=CARTESIAN_POINT('Ctrl Pts',(-7.70627967396427,0.147859670634715,
-0.617300284420033));
#12967=CARTESIAN_POINT('Ctrl Pts',(-7.44563117789263,0.337027277983696,
-0.633000297155258));
#12968=CARTESIAN_POINT('Ctrl Pts',(-7.14406470060242,0.223979898328531,
-0.648700309890483));
#12969=CARTESIAN_POINT('Ctrl Pts',(-7.07199799524557,-0.0899136284440642,
-0.664400322625708));
#12970=CARTESIAN_POINT('Ctrl Pts',(-7.29405356466082,-0.323178273560057,
-0.680100335360934));
#12971=CARTESIAN_POINT('Ctrl Pts',(-7.61111286296356,-0.266650840389621,
-0.695800348096159));
#12972=CARTESIAN_POINT('Ctrl Pts',(-7.73886413438061,0.0289950066804033,
-0.711500360831385));
#12973=CARTESIAN_POINT('Ctrl Pts',(-7.56275489944635,0.298620482975957,
-0.72720037356661));
#12974=CARTESIAN_POINT('Ctrl Pts',(-7.24069731847952,0.300511002471844,
-0.742900386301835));
#12975=CARTESIAN_POINT('Ctrl Pts',(-7.06149698883364,0.0328479119748854,
-0.75860039903706));
#12976=CARTESIAN_POINT('Ctrl Pts',(-7.18581741009011,-0.264103673257608,
-0.774300411772286));
#12977=CARTESIAN_POINT('Ctrl Pts',(-7.5022335053935,-0.324568202559814,
-0.790000424507511));
#12978=CARTESIAN_POINT('Ctrl Pts',(-7.7269066182366,-0.0932950686654655,
-0.805700437242737));
#12979=CARTESIAN_POINT('Ctrl Pts',(-7.68123478989901,0.11550380736018,-0.816167112399554));
#12980=CARTESIAN_POINT('Ctrl Pts',(-7.61951971040191,0.187686343907874,
-0.821400449977962));
#12981=CARTESIAN_POINT('Ctrl Pts',(-7.4698066426161,-0.261113218593861,
0.0214004499779621));
#12982=CARTESIAN_POINT('Ctrl Pts',(-7.55566596891409,-0.2381593775803,0.0161671123995537));
#12983=CARTESIAN_POINT('Ctrl Pts',(-7.70157179612354,-0.101339947425821,
0.00570043724273678));
#12984=CARTESIAN_POINT('Ctrl Pts',(-7.65089580253497,0.196120032593032,
-0.00999957549248853));
#12985=CARTESIAN_POINT('Ctrl Pts',(-7.37481774109234,0.317218576489643,
-0.0256995882277139));
#12986=CARTESIAN_POINT('Ctrl Pts',(-7.12152745620743,0.154105135308149,
-0.0413996009629392));
#12987=CARTESIAN_POINT('Ctrl Pts',(-7.1178438945145,-0.14731468094579,-0.0570996136981647));
#12988=CARTESIAN_POINT('Ctrl Pts',(-7.36722310560002,-0.316577150710778,
-0.0727996264333899));
#12989=CARTESIAN_POINT('Ctrl Pts',(-7.64596854962699,-0.20199102388638,
-0.0884996391686153));
#12990=CARTESIAN_POINT('Ctrl Pts',(-7.70416408791058,0.0937368510268085,
-0.104199651903841));
#12991=CARTESIAN_POINT('Ctrl Pts',(-7.48960659831061,0.305402825458584,
-0.119899664639066));
#12992=CARTESIAN_POINT('Ctrl Pts',(-7.19470107172442,0.243214708783014,
-0.135599677374291));
#12993=CARTESIAN_POINT('Ctrl Pts',(-7.08388754724896,-0.0370681313492207,
-0.151299690109517));
#12994=CARTESIAN_POINT('Ctrl Pts',(-7.25653584343968,-0.284110749719476,
-0.166999702844742));
#12995=CARTESIAN_POINT('Ctrl Pts',(-7.55782945258926,-0.276388965781158,
-0.182699715579967));
#12996=CARTESIAN_POINT('Ctrl Pts',(-7.71759606212085,-0.0208263302462058,
-0.198399728315193));
#12997=CARTESIAN_POINT('Ctrl Pts',(-7.59257114433741,0.253411369136158,
-0.214099741050418));
#12998=CARTESIAN_POINT('Ctrl Pts',(-7.29486587935229,0.300412715376446,
-0.229799753785643));
#12999=CARTESIAN_POINT('Ctrl Pts',(-7.09143536647491,0.078031071597451,
-0.245499766520869));
#13000=CARTESIAN_POINT('Ctrl Pts',(-7.16469773186114,-0.214321769736272,
-0.261199779256094));
#13001=CARTESIAN_POINT('Ctrl Pts',(-7.44895789295024,-0.314490230452922,
-0.276899791991319));
#13002=CARTESIAN_POINT('Ctrl Pts',(-7.68931704448864,-0.132652281259804,
-0.292599804726545));
#13003=CARTESIAN_POINT('Ctrl Pts',(-7.67024282529466,0.168136239570967,
-0.30829981746177));
#13004=CARTESIAN_POINT('Ctrl Pts',(-7.40883927273945,0.318155382134106,
-0.323999830196995));
#13005=CARTESIAN_POINT('Ctrl Pts',(-7.13950945918524,0.182881540904911,
-0.339699842932221));
#13006=CARTESIAN_POINT('Ctrl Pts',(-7.10376401277782,-0.116383932345987,
-0.355399855667446));
#13007=CARTESIAN_POINT('Ctrl Pts',(-7.33365621799037,-0.311286817024221,
-0.371099868402672));
#13008=CARTESIAN_POINT('Ctrl Pts',(-7.62303952904418,-0.227055826471647,
-0.386799881137896));
#13009=CARTESIAN_POINT('Ctrl Pts',(-7.71242115464125,0.0607783019144452,
-0.402499893873122));
#13010=CARTESIAN_POINT('Ctrl Pts',(-7.52165173364529,0.294111943935478,
-0.418199906608347));
#13011=CARTESIAN_POINT('Ctrl Pts',(-7.22179603601754,0.263712584179732,
-0.433899919343573));
#13012=CARTESIAN_POINT('Ctrl Pts',(-7.08173754249308,-0.00316037962629422,
-0.449599932078798));
#13013=CARTESIAN_POINT('Ctrl Pts',(-7.22706804791315,-0.267199400955335,
-0.465299944814023));
#13014=CARTESIAN_POINT('Ctrl Pts',(-7.52746829374862,-0.291638155544021,
-0.480999957549249));
#13015=CARTESIAN_POINT('Ctrl Pts',(-7.71356649781592,-0.0545621792318911,
-0.496699970284474));
#13016=CARTESIAN_POINT('Ctrl Pts',(-7.61848661484522,0.231440228711292,
-0.512399983019699));
#13017=CARTESIAN_POINT('Ctrl Pts',(-7.3274876887327,0.309907959060197,-0.528099995754925));
#13018=CARTESIAN_POINT('Ctrl Pts',(-7.10151124686598,0.110478257814012,
-0.54380000849015));
#13019=CARTESIAN_POINT('Ctrl Pts',(-7.1431925353605,-0.188018374074586,
-0.559500021225376));
#13020=CARTESIAN_POINT('Ctrl Pts',(-7.41515553735499,-0.31791709190662,
-0.575200033960601));
#13021=CARTESIAN_POINT('Ctrl Pts',(-7.67352843115613,-0.162736572581166,
-0.590900046695826));
#13022=CARTESIAN_POINT('Ctrl Pts',(-7.68662574139757,0.138371532037808,
-0.606600059431052));
#13023=CARTESIAN_POINT('Ctrl Pts',(-7.44270303028938,0.315400275091557,
-0.622300072166277));
#13024=CARTESIAN_POINT('Ctrl Pts',(-7.16048804026023,0.209607133198326,
-0.638000084901502));
#13025=CARTESIAN_POINT('Ctrl Pts',(-7.09304584735977,-0.0841438809208489,
-0.653700097636728));
#13026=CARTESIAN_POINT('Ctrl Pts',(-7.30085213561686,-0.302439959739364,
-0.669400110371953));
#13027=CARTESIAN_POINT('Ctrl Pts',(-7.59756577405967,-0.249539885659789,
-0.685100123107178));
#13028=CARTESIAN_POINT('Ctrl Pts',(-7.71711926061806,0.0271344003310113,
-0.700800135842403));
#13029=CARTESIAN_POINT('Ctrl Pts',(-7.55231093567554,0.279458039841947,
-0.716500148577629));
#13030=CARTESIAN_POINT('Ctrl Pts',(-7.25091975381051,0.281227244912337,
-0.732200161312854));
#13031=CARTESIAN_POINT('Ctrl Pts',(-7.08321868935976,0.0307400651218602,
-0.74790017404808));
#13032=CARTESIAN_POINT('Ctrl Pts',(-7.19956148303025,-0.247156169958949,
-0.763600186783305));
#13033=CARTESIAN_POINT('Ctrl Pts',(-7.49567319273855,-0.303740697150009,
-0.77930019951853));
#13034=CARTESIAN_POINT('Ctrl Pts',(-7.70592905695325,-0.0873083344998472,
-0.795000212253755));
#13035=CARTESIAN_POINT('Ctrl Pts',(-7.66318798475343,0.108091940905998,
-0.805466887410572));
#13036=CARTESIAN_POINT('Ctrl Pts',(-7.60543315503421,0.175642532122684,
-0.810700224988981));
#13037=CARTESIAN_POINT('Ctrl Pts',(-7.46501999979751,-0.243208680203507,
0.0321006749669432));
#13038=CARTESIAN_POINT('Ctrl Pts',(-7.54499195044998,-0.221828784507026,
0.0268673373885347));
#13039=CARTESIAN_POINT('Ctrl Pts',(-7.68089301229858,-0.094391065293644,
0.0164006622317178));
#13040=CARTESIAN_POINT('Ctrl Pts',(-7.6336918725591,0.182672078209147,0.000700649496492535));
#13041=CARTESIAN_POINT('Ctrl Pts',(-7.37654448906701,0.295466892635879,
-0.0149993632387329));
#13042=CARTESIAN_POINT('Ctrl Pts',(-7.1406223238585,0.143538143234235,-0.0306993759739581));
#13043=CARTESIAN_POINT('Ctrl Pts',(-7.13719134406127,-0.137213310457307,
-0.0463993887091836));
#13044=CARTESIAN_POINT('Ctrl Pts',(-7.36947061787559,-0.294869449434932,
-0.0620994014444088));
#13045=CARTESIAN_POINT('Ctrl Pts',(-7.62910248147719,-0.188140495517282,
-0.0777994141796343));
#13046=CARTESIAN_POINT('Ctrl Pts',(-7.68330755058823,0.0873093133600507,
-0.0934994269148595));
#13047=CARTESIAN_POINT('Ctrl Pts',(-7.48346227215155,0.284461347878887,
-0.109199439650085));
#13048=CARTESIAN_POINT('Ctrl Pts',(-7.20877842316073,0.226537471552532,
-0.12489945238531));
#13049=CARTESIAN_POINT('Ctrl Pts',(-7.10556338417682,-0.0345263688740197,
-0.140599465120536));
#13050=CARTESIAN_POINT('Ctrl Pts',(-7.26637318339745,-0.264629270180224,
-0.156299477855761));
#13051=CARTESIAN_POINT('Ctrl Pts',(-7.54700708400818,-0.257436969114164,
-0.171999490590986));
#13052=CARTESIAN_POINT('Ctrl Pts',(-7.69581849407014,-0.0193982683831129,
-0.187699503326212));
#13053=CARTESIAN_POINT('Ctrl Pts',(-7.57936653728905,0.236034946710346,
-0.203399516061437));
#13054=CARTESIAN_POINT('Ctrl Pts',(-7.30207492801482,0.279813409740471,
-0.219099528796662));
#13055=CARTESIAN_POINT('Ctrl Pts',(-7.11259364929416,0.0726804795263919,
-0.234799541531888));
#13056=CARTESIAN_POINT('Ctrl Pts',(-7.1808324128854,-0.199625721888536,
-0.250499554267113));
#13057=CARTESIAN_POINT('Ctrl Pts',(-7.44560084929478,-0.292925629339051,
-0.266199567002339));
#13058=CARTESIAN_POINT('Ctrl Pts',(-7.66947856921755,-0.123556311798072,
-0.281899579737563));
#13059=CARTESIAN_POINT('Ctrl Pts',(-7.65171226959831,0.156607134409536,
-0.297599592472789));
#13060=CARTESIAN_POINT('Ctrl Pts',(-7.40823316363873,0.296339461499394,
-0.313299605208014));
#13061=CARTESIAN_POINT('Ctrl Pts',(-7.15737130054838,0.170341350149144,
-0.32899961794324));
#13062=CARTESIAN_POINT('Ctrl Pts',(-7.12407692008441,-0.108403483880257,
-0.344699630678465));
#13063=CARTESIAN_POINT('Ctrl Pts',(-7.33820541239099,-0.289941874030391,
-0.360399643413691));
#13064=CARTESIAN_POINT('Ctrl Pts',(-7.60774570427405,-0.211486604110145,
-0.376099656148916));
#13065=CARTESIAN_POINT('Ctrl Pts',(-7.69099843009533,0.0566107325903492,
-0.391799668884141));
#13066=CARTESIAN_POINT('Ctrl Pts',(-7.51331007194377,0.273944682317654,
-0.407499681619366));
#13067=CARTESIAN_POINT('Ctrl Pts',(-7.23401548523432,0.245629807241466,
-0.423199694354592));
#13068=CARTESIAN_POINT('Ctrl Pts',(-7.10356080528816,-0.00294367233490627,
-0.438899707089817));
#13069=CARTESIAN_POINT('Ctrl Pts',(-7.23892599517347,-0.248877532924113,
-0.454599719825043));
#13070=CARTESIAN_POINT('Ctrl Pts',(-7.51872779040962,-0.271640521643488,
-0.470299732560268));
#13071=CARTESIAN_POINT('Ctrl Pts',(-7.69206523706663,-0.0508208495589636,
-0.485999745295494));
#13072=CARTESIAN_POINT('Ctrl Pts',(-7.60350498348874,0.215570367804407,
-0.501699758030718));
#13073=CARTESIAN_POINT('Ctrl Pts',(-7.33245985930243,0.288657564383319,
-0.517399770765944));
#13074=CARTESIAN_POINT('Ctrl Pts',(-7.12197862637422,0.102902761563831,
-0.533099783501169));
#13075=CARTESIAN_POINT('Ctrl Pts',(-7.1608018281199,-0.175125950570181,
-0.548799796236394));
#13076=CARTESIAN_POINT('Ctrl Pts',(-7.41411632186885,-0.296117510837361,
-0.56449980897162));
#13077=CARTESIAN_POINT('Ctrl Pts',(-7.65477258140305,-0.151577722688444,
-0.580199821706845));
#13078=CARTESIAN_POINT('Ctrl Pts',(-7.66697180883088,0.128883393440901,
-0.59589983444207));
#13079=CARTESIAN_POINT('Ctrl Pts',(-7.43977488268614,0.293773272199418,
-0.611599847177296));
#13080=CARTESIAN_POINT('Ctrl Pts',(-7.17691137991803,0.195234368068121,
-0.627299859912521));
#13081=CARTESIAN_POINT('Ctrl Pts',(-7.11409369947397,-0.0783741333976333,
-0.642999872647747));
#13082=CARTESIAN_POINT('Ctrl Pts',(-7.30765070657289,-0.281701645918672,
-0.658699885382972));
#13083=CARTESIAN_POINT('Ctrl Pts',(-7.58401868515578,-0.232428930929957,
-0.674399898118197));
#13084=CARTESIAN_POINT('Ctrl Pts',(-7.69537438685551,0.0252737939816199,
-0.690099910853423));
#13085=CARTESIAN_POINT('Ctrl Pts',(-7.54186697190474,0.260295596707937,
-0.705799923588648));
#13086=CARTESIAN_POINT('Ctrl Pts',(-7.2611421891415,0.261943487352831,-0.721499936323873));
#13087=CARTESIAN_POINT('Ctrl Pts',(-7.10494038988587,0.028632218268835,
-0.737199949059099));
#13088=CARTESIAN_POINT('Ctrl Pts',(-7.2133055559704,-0.23020866666029,-0.752899961794324));
#13089=CARTESIAN_POINT('Ctrl Pts',(-7.4891128800836,-0.282913191740204,
-0.76859997452955));
#13090=CARTESIAN_POINT('Ctrl Pts',(-7.68495149566991,-0.0813216003342288,
-0.784299987264774));
#13091=CARTESIAN_POINT('Ctrl Pts',(-7.64514117960785,0.100680074451816,
-0.794766662421591));
#13092=CARTESIAN_POINT('Ctrl Pts',(-7.59134659966651,0.163598720337494,
-0.8));
#13093=CARTESIAN_POINT('Ctrl Pts',(-7.65159361924534,0.000201202514259572,
-0.0887416697508019));
#13094=CARTESIAN_POINT('Ctrl Pts',(-7.65178908806815,0.0253219403653002,
-0.0903275888054878));
#13095=CARTESIAN_POINT('Ctrl Pts',(-7.64832166662565,0.0503900135757667,
-0.0919135078601737));
#13096=CARTESIAN_POINT('Ctrl Pts',(-7.64096582599694,0.0742596843003013,
-0.0934994269148595));
#13097=CARTESIAN_POINT('Ctrl Pts',(-7.616692457776,0.153026658199663,-0.098732764493268));
#13098=CARTESIAN_POINT('Ctrl Pts',(-7.55007736496378,0.218744003039275,
-0.103966102071676));
#13099=CARTESIAN_POINT('Ctrl Pts',(-7.4709891770592,0.241948696071355,-0.109199439650085));
#13100=CARTESIAN_POINT('Ctrl Pts',(-7.39190098915461,0.265153389103436,
-0.114432777228493));
#13101=CARTESIAN_POINT('Ctrl Pts',(-7.30033970615767,0.245845430327984,
-0.119666114806902));
#13102=CARTESIAN_POINT('Ctrl Pts',(-7.23735655816188,0.192680810869166,
-0.12489945238531));
#13103=CARTESIAN_POINT('Ctrl Pts',(-7.17437341016609,0.139516191410348,
-0.130132789963719));
#13104=CARTESIAN_POINT('Ctrl Pts',(-7.13996839717146,0.0524949112681644,
-0.135366127542127));
#13105=CARTESIAN_POINT('Ctrl Pts',(-7.14956752387758,-0.0293662123539616,
-0.140599465120536));
#13106=CARTESIAN_POINT('Ctrl Pts',(-7.1591666505837,-0.111227335976088,
-0.145832802698944));
#13107=CARTESIAN_POINT('Ctrl Pts',(-7.21276991699057,-0.187928303078155,
-0.151066140277352));
#13108=CARTESIAN_POINT('Ctrl Pts',(-7.28634386696247,-0.225080069784846,
-0.156299477855761));
#13109=CARTESIAN_POINT('Ctrl Pts',(-7.35991781693436,-0.262231836491537,
-0.161532815434169));
#13110=CARTESIAN_POINT('Ctrl Pts',(-7.45346245047127,-0.25983440280285,
-0.166766153012578));
#13111=CARTESIAN_POINT('Ctrl Pts',(-7.52503666891672,-0.218962569169999,
-0.171999490590986));
#13112=CARTESIAN_POINT('Ctrl Pts',(-7.59661088736217,-0.178090735537147,
-0.177232828169395));
#13113=CARTESIAN_POINT('Ctrl Pts',(-7.64621469071615,-0.0987445019601298,
-0.182466165747803));
#13114=CARTESIAN_POINT('Ctrl Pts',(-7.65160793292963,-0.016499182656045,
-0.187699503326212));
#13115=CARTESIAN_POINT('Ctrl Pts',(-7.65196593620322,-0.0110397405648857,
-0.188046892134408));
#13116=CARTESIAN_POINT('Ctrl Pts',(-7.65212913444403,-0.00556752422984645,
-0.188394280942605));
#13117=CARTESIAN_POINT('Ctrl Pts',(-7.65210261813639,-9.36994259479408E-5,
-0.188741669750802));
#13118=CARTESIAN_POINT('Ctrl Pts',(-7.47937992825329,-0.29692229537457,
0.));
#13119=CARTESIAN_POINT('Ctrl Pts',(-7.49619114386871,-0.290772677607239,
-8.69477011477833E-19));
#13120=CARTESIAN_POINT('Ctrl Pts',(-7.51233082429301,-0.283071243582746,
-2.76754902901489E-17));
#13121=CARTESIAN_POINT('Ctrl Pts',(-7.52766936287682,-0.274000229956832,
-3.51281503885303E-17));
#13122=CARTESIAN_POINT('Ctrl Pts',(-7.53764505481519,-0.268100734577494,
-3.99751207082049E-17));
#13123=CARTESIAN_POINT('Ctrl Pts',(-7.5472814350885,-0.261620842282721,
9.85568025155778E-18));
#13124=CARTESIAN_POINT('Ctrl Pts',(-7.55653522793476,-0.254602062866676,
1.64798730217797E-17));
#13125=CARTESIAN_POINT('Ctrl Pts',(-7.56394892482147,-0.248978952000698,
2.1786859911754E-17));
#13126=CARTESIAN_POINT('Ctrl Pts',(-7.57111696210311,-0.243009806706639,
1.89150345061034E-17));
#13127=CARTESIAN_POINT('Ctrl Pts',(-7.57801342324538,-0.236714009089512,
2.86229373536173E-17));
#13128=CARTESIAN_POINT('Ctrl Pts',(-7.58154042561042,-0.233494199301952,
3.35877730275079E-17));
#13129=CARTESIAN_POINT('Ctrl Pts',(-7.58499006695748,-0.23019457260616,
-3.76648489097615E-18));
#13130=CARTESIAN_POINT('Ctrl Pts',(-7.5883566289172,-0.226821418549513,
8.67361737988404E-19));
#13131=CARTESIAN_POINT('Ctrl Pts',(-7.60071585533099,-0.21443799141716,
1.78790075474068E-17));
#13132=CARTESIAN_POINT('Ctrl Pts',(-7.61197268590976,-0.201052893031173,
4.33275306678286E-18));
#13133=CARTESIAN_POINT('Ctrl Pts',(-7.62197690688824,-0.186813942786284,
1.04083408558608E-17));
#13134=CARTESIAN_POINT('Ctrl Pts',(-7.62826586469373,-0.177862905271498,
1.42276402627068E-17));
#13135=CARTESIAN_POINT('Ctrl Pts',(-7.63405901293069,-0.168573843374886,
-1.87641832666448E-17));
#13136=CARTESIAN_POINT('Ctrl Pts',(-7.63930885204487,-0.158980190860473,
-2.60208521396521E-17));
#13137=CARTESIAN_POINT('Ctrl Pts',(-7.64155361520625,-0.154878069389871,
-2.9123709695134E-17));
#13138=CARTESIAN_POINT('Ctrl Pts',(-7.64369893607691,-0.150720243293487,
-2.44962438590674E-18));
#13139=CARTESIAN_POINT('Ctrl Pts',(-7.64574058754886,-0.146509291490871,
0.));
#13140=CARTESIAN_POINT('Ctrl Pts',(-7.64768690274554,-0.142494972887256,
2.3352375437085E-18));
#13141=CARTESIAN_POINT('Ctrl Pts',(-7.6495350879677,-0.138440370831646,
-9.39867744994685E-18));
#13142=CARTESIAN_POINT('Ctrl Pts',(-7.65128174628091,-0.134349965575425,
-6.93889390390723E-18));
#13143=CARTESIAN_POINT('Ctrl Pts',(-7.65753758940913,-0.11969974267822,
1.87108334065775E-18));
#13144=CARTESIAN_POINT('Ctrl Pts',(-7.66249839256794,-0.104582615525194,
3.46944695195361E-18));
#13145=CARTESIAN_POINT('Ctrl Pts',(-7.66602473772058,-0.0891085568120877,
3.46944695195361E-18));
#13146=CARTESIAN_POINT('Ctrl Pts',(-7.66854165586043,-0.0780639944149697,
-3.18384531345276E-19));
#13147=CARTESIAN_POINT('Ctrl Pts',(-7.67032673519256,-0.0668371954593955,
-2.99514844422014E-17));
#13148=CARTESIAN_POINT('Ctrl Pts',(-7.67139185115297,-0.0554969491587786,
-3.12250225675825E-17));
#13149=CARTESIAN_POINT('Ctrl Pts',(-7.67180517284341,-0.0510963299350149,
-3.17192231526653E-17));
#13150=CARTESIAN_POINT('Ctrl Pts',(-7.67210997162644,-0.0466786569219802,
1.16129547820002E-17));
#13151=CARTESIAN_POINT('Ctrl Pts',(-7.67230655013972,-0.0422481088180091,
1.04083408558608E-17));
#13152=CARTESIAN_POINT('Ctrl Pts',(-7.6725090500926,-0.0376841014537716,
9.16744092633848E-18));
#13153=CARTESIAN_POINT('Ctrl Pts',(-7.67259625011215,-0.0331162258874048,
8.24472046592442E-18));
#13154=CARTESIAN_POINT('Ctrl Pts',(-7.67256982465584,-0.0285510304520631,
1.04083408558608E-17));
#13155=CARTESIAN_POINT('Ctrl Pts',(-7.67247174711471,-0.0116074008728858,
1.84385737245866E-17));
#13156=CARTESIAN_POINT('Ctrl Pts',(-7.6708130923532,0.00531022346404731,
1.85851794107315E-17));
#13157=CARTESIAN_POINT('Ctrl Pts',(-7.66764846010905,0.0219708181576634,
3.46944695195361E-18));
#13158=CARTESIAN_POINT('Ctrl Pts',(-7.66599431782927,0.0306792531235465,
-4.43149389077601E-18));
#13159=CARTESIAN_POINT('Ctrl Pts',(-7.66392781727349,0.0393172333562807,
-5.69158656397132E-18));
#13160=CARTESIAN_POINT('Ctrl Pts',(-7.66145136629352,0.0478487584034829,
-3.46944695195361E-18));
#13161=CARTESIAN_POINT('Ctrl Pts',(-7.66000105406562,0.0528451727071283,
-2.16806999053646E-18));
#13162=CARTESIAN_POINT('Ctrl Pts',(-7.65840948355064,0.0578066853598702,
-4.88676934904438E-17));
#13163=CARTESIAN_POINT('Ctrl Pts',(-7.6566784834973,0.0627203082789222,
-2.42861286636753E-17));
#13164=CARTESIAN_POINT('Ctrl Pts',(-7.65135793333965,0.077823240913812,
5.12698762953888E-17));
#13165=CARTESIAN_POINT('Ctrl Pts',(-7.64474871423961,0.0924063141758472,
-3.57806052195261E-17));
#13166=CARTESIAN_POINT('Ctrl Pts',(-7.63687440208771,0.106254953674968,
-3.12250225675825E-17));
#13167=CARTESIAN_POINT('Ctrl Pts',(-7.63280782486428,0.113406887821882,
-2.88723562908995E-17));
#13168=CARTESIAN_POINT('Ctrl Pts',(-7.62839916570184,0.12036724850192,5.48664495430319E-17));
#13169=CARTESIAN_POINT('Ctrl Pts',(-7.62366911690659,0.127074854237358,
3.12250225675825E-17));
#13170=CARTESIAN_POINT('Ctrl Pts',(-7.61642299052403,0.137350468927051,
-4.9921022748546E-18));
#13171=CARTESIAN_POINT('Ctrl Pts',(-7.60841822005153,0.147045784154728,
-4.13752983739663E-17));
#13172=CARTESIAN_POINT('Ctrl Pts',(-7.59965866901871,0.156042617987613,
-3.46944695195361E-17));
#13173=CARTESIAN_POINT('Ctrl Pts',(-7.59707213175836,0.158699220574521,
-3.26179135892075E-17));
#13174=CARTESIAN_POINT('Ctrl Pts',(-7.59441969136407,0.161294781931434,
-1.60581715346596E-17));
#13175=CARTESIAN_POINT('Ctrl Pts',(-7.59170406260212,0.16382811505057,-1.38777878078145E-17));
#13176=CARTESIAN_POINT('Origin',(7.4,0.,0.220842344717745));
#13177=CARTESIAN_POINT('Ctrl Pts',(7.09227939521384,0.000154311006394908,
-0.0291576552822542));
#13178=CARTESIAN_POINT('Ctrl Pts',(7.09221571350587,0.0100435698963641,
-0.0296715621794889));
#13179=CARTESIAN_POINT('Ctrl Pts',(7.09709968515426,0.120578449441071,-0.035418806655132));
#13180=CARTESIAN_POINT('Ctrl Pts',(7.23047491327011,0.319794756266977,-0.0463993887091836));
#13181=CARTESIAN_POINT('Ctrl Pts',(7.5731988395346,0.317782877693097,-0.0620994014444088));
#13182=CARTESIAN_POINT('Ctrl Pts',(7.76060897472171,0.0308556191331042,
-0.0777994141796343));
#13183=CARTESIAN_POINT('Ctrl Pts',(7.62465992779684,-0.283761771610304,
-0.0934994269148594));
#13184=CARTESIAN_POINT('Ctrl Pts',(7.2872550057463,-0.343916549876741,-0.109199439650085));
#13185=CARTESIAN_POINT('Ctrl Pts',(7.10835469415216,-0.155985587810117,
-0.12108551577255));
#13186=CARTESIAN_POINT('Ctrl Pts',(7.09252332370173,-0.0276893492462785,
-0.127738254316606));
#13187=CARTESIAN_POINT('Ctrl Pts',(7.09275435891078,-0.000260665786541426,
-0.129157655282254));
#13188=CARTESIAN_POINT('Ctrl Pts',(7.09298021495369,-0.000306384811325677,
-0.0208423447177452));
#13189=CARTESIAN_POINT('Ctrl Pts',(7.09344513148094,0.0677879045700394,
-0.0243615716353137));
#13190=CARTESIAN_POINT('Ctrl Pts',(7.14897196854486,0.238050685086685,-0.0331141361312906));
#13191=CARTESIAN_POINT('Ctrl Pts',(7.42863574892529,0.360721777030891,-0.047100038205676));
#13192=CARTESIAN_POINT('Ctrl Pts',(7.71666223333994,0.175239166203998,-0.0628000509409013));
#13193=CARTESIAN_POINT('Ctrl Pts',(7.72085097116846,-0.167517439243982,
-0.0785000636761268));
#13194=CARTESIAN_POINT('Ctrl Pts',(7.43727190914667,-0.359992487166362,
-0.094200076411352));
#13195=CARTESIAN_POINT('Ctrl Pts',(7.15231797731739,-0.242854213543255,
-0.108314170091892));
#13196=CARTESIAN_POINT('Ctrl Pts',(7.09338979712027,-0.0702887118513222,
-0.117194926194023));
#13197=CARTESIAN_POINT('Ctrl Pts',(7.09284095646985,0.000245638412278346,
-0.120842344717745));
#13198=CARTESIAN_POINT('Ctrl Pts',(7.59134659966651,0.163598720337495,0.));
#13199=CARTESIAN_POINT('Ctrl Pts',(7.64514117960785,0.100680074451818,-0.00523333757840845));
#13200=CARTESIAN_POINT('Ctrl Pts',(7.68495172974597,-0.0813213515576848,
-0.0157000127352253));
#13201=CARTESIAN_POINT('Ctrl Pts',(7.48911277275958,-0.282913268514194,
-0.0314000254704507));
#13202=CARTESIAN_POINT('Ctrl Pts',(7.213305621753,-0.230208577870288,-0.047100038205676));
#13203=CARTESIAN_POINT('Ctrl Pts',(7.10494039731525,0.0286321757004985,
-0.0628000509409014));
#13204=CARTESIAN_POINT('Ctrl Pts',(7.26114221381406,0.261943484269437,-0.0785000636761267));
#13205=CARTESIAN_POINT('Ctrl Pts',(7.54186695250638,0.260295557049739,-0.094200076411352));
#13206=CARTESIAN_POINT('Ctrl Pts',(7.69537435948004,0.0252737989808328,
-0.109900089146577));
#13207=CARTESIAN_POINT('Ctrl Pts',(7.58401866543957,-0.232428911673642,
-0.125600101881803));
#13208=CARTESIAN_POINT('Ctrl Pts',(7.30765071643609,-0.281701615199185,
-0.141300114617028));
#13209=CARTESIAN_POINT('Ctrl Pts',(7.11409372805788,-0.0783741267420522,
-0.157000127352254));
#13210=CARTESIAN_POINT('Ctrl Pts',(7.17691140254618,0.195234349047302,-0.172700140087479));
#13211=CARTESIAN_POINT('Ctrl Pts',(7.43977487861582,0.293773242201156,-0.188400152822704));
#13212=CARTESIAN_POINT('Ctrl Pts',(7.66697178192527,0.128883380631593,-0.204100165557929));
#13213=CARTESIAN_POINT('Ctrl Pts',(7.65477255568824,-0.15157770749914,-0.219800178293155));
#13214=CARTESIAN_POINT('Ctrl Pts',(7.41411632045071,-0.29611748091033,-0.23550019102838));
#13215=CARTESIAN_POINT('Ctrl Pts',(7.16080185224803,-0.175125932931451,
-0.251200203763606));
#13216=CARTESIAN_POINT('Ctrl Pts',(7.12197865442297,0.102902751197641,-0.266900216498831));
#13217=CARTESIAN_POINT('Ctrl Pts',(7.33245986611545,0.288657535255061,-0.282600229234056));
#13218=CARTESIAN_POINT('Ctrl Pts',(7.60350496295894,0.215570346061205,-0.298300241969282));
#13219=CARTESIAN_POINT('Ctrl Pts',(7.69206520760226,-0.050820844434144,
-0.314000254704507));
#13220=CARTESIAN_POINT('Ctrl Pts',(7.51872777843214,-0.271640494238638,
-0.329700267439732));
#13221=CARTESIAN_POINT('Ctrl Pts',(7.23892601142296,-0.248877507817314,
-0.345400280174957));
#13222=CARTESIAN_POINT('Ctrl Pts',(7.10356083519368,-0.00294367203764689,
-0.361100292910183));
#13223=CARTESIAN_POINT('Ctrl Pts',(7.23401550197922,0.245629782461581,-0.376800305645408));
#13224=CARTESIAN_POINT('Ctrl Pts',(7.51331006051279,0.273944654681539,-0.392500318380634));
#13225=CARTESIAN_POINT('Ctrl Pts',(7.69099840073869,0.0566107268792646,
-0.408200331115859));
#13226=CARTESIAN_POINT('Ctrl Pts',(7.60774568331619,-0.21148658277481,-0.423900343851084));
#13227=CARTESIAN_POINT('Ctrl Pts',(7.33820541862493,-0.28994184478043,-0.43960035658631));
#13228=CARTESIAN_POINT('Ctrl Pts',(7.12407694792028,-0.108403472944119,
-0.455300369321535));
#13229=CARTESIAN_POINT('Ctrl Pts',(7.15737132502519,0.170341332964446,-0.47100038205676));
#13230=CARTESIAN_POINT('Ctrl Pts',(7.40823316280845,0.296339431604435,-0.486700394791985));
#13231=CARTESIAN_POINT('Ctrl Pts',(7.6517122442044,0.156607118609695,-0.502400407527211));
#13232=CARTESIAN_POINT('Ctrl Pts',(7.66947854203298,-0.123556299331602,
-0.518100420262436));
#13233=CARTESIAN_POINT('Ctrl Pts',(7.44560084469238,-0.292925599791504,
-0.533800432997662));
#13234=CARTESIAN_POINT('Ctrl Pts',(7.18083243499946,-0.199625701743059,
-0.549500445732886));
#13235=CARTESIAN_POINT('Ctrl Pts',(7.11259367828104,0.0726804721812103,
-0.565200458468113));
#13236=CARTESIAN_POINT('Ctrl Pts',(7.30207493790754,0.27981338153719,-0.580900471203337));
#13237=CARTESIAN_POINT('Ctrl Pts',(7.57936651916845,0.236034922850711,-0.596600483938564));
#13238=CARTESIAN_POINT('Ctrl Pts',(7.69581846427466,-0.0193982663347125,
-0.612300496673787));
#13239=CARTESIAN_POINT('Ctrl Pts',(7.54700706909094,-0.257436943317534,
-0.628000509409014));
#13240=CARTESIAN_POINT('Ctrl Pts',(7.26637319703535,-0.264629243152998,
-0.643700522144239));
#13241=CARTESIAN_POINT('Ctrl Pts',(7.1055634135989,-0.0345263660164505,
-0.659400534879464));
#13242=CARTESIAN_POINT('Ctrl Pts',(7.20877844294678,0.226537449876541,-0.67510054761469));
#13243=CARTESIAN_POINT('Ctrl Pts',(7.48346226287904,0.284461316975979,-0.690800560349915));
#13244=CARTESIAN_POINT('Ctrl Pts',(7.68330752343249,0.0873093086589616,
-0.706500573085141));
#13245=CARTESIAN_POINT('Ctrl Pts',(7.62910245608525,-0.188140484130538,
-0.722200585820366));
#13246=CARTESIAN_POINT('Ctrl Pts',(7.36947062435342,-0.294869405764503,
-0.737900598555591));
#13247=CARTESIAN_POINT('Ctrl Pts',(7.13719136614053,-0.137213321891836,
-0.753600611290817));
#13248=CARTESIAN_POINT('Ctrl Pts',(7.14062235409354,0.143538174106571,-0.769300624026041));
#13249=CARTESIAN_POINT('Ctrl Pts',(7.37654449298423,0.295466782201871,-0.785000636761268));
#13250=CARTESIAN_POINT('Ctrl Pts',(7.63369182760114,0.182672202271517,-0.800700649496493));
#13251=CARTESIAN_POINT('Ctrl Pts',(7.68089306428376,-0.0943914029012692,
-0.816400662231718));
#13252=CARTESIAN_POINT('Ctrl Pts',(7.54499195044998,-0.221828784507026,
-0.826867337388535));
#13253=CARTESIAN_POINT('Ctrl Pts',(7.46501999979751,-0.243208680203507,
-0.832100674966943));
#13254=CARTESIAN_POINT('Ctrl Pts',(7.60543315503421,0.175642532122685,0.0107002249889811));
#13255=CARTESIAN_POINT('Ctrl Pts',(7.66318798475343,0.108091940906,0.00546688741057261));
#13256=CARTESIAN_POINT('Ctrl Pts',(7.70592930826152,-0.0873080674088697,
-0.00499978774624429));
#13257=CARTESIAN_POINT('Ctrl Pts',(7.49567307751356,-0.303740779575947,
-0.0206998004814696));
#13258=CARTESIAN_POINT('Ctrl Pts',(7.19956155365563,-0.247156074632404,
-0.036399813216695));
#13259=CARTESIAN_POINT('Ctrl Pts',(7.08321869733608,0.0307400194197276,
-0.0520998259519203));
#13260=CARTESIAN_POINT('Ctrl Pts',(7.25091978029941,0.28122724160195,-0.0677998386871457));
#13261=CARTESIAN_POINT('Ctrl Pts',(7.55231091484912,0.279457997264192,-0.083499851422371));
#13262=CARTESIAN_POINT('Ctrl Pts',(7.71711923122726,0.0271344056982565,
-0.0991998641575963));
#13263=CARTESIAN_POINT('Ctrl Pts',(7.597565752892,-0.249539864985863,-0.114899876892822));
#13264=CARTESIAN_POINT('Ctrl Pts',(7.30085214620616,-0.302439926758371,
-0.130599889628047));
#13265=CARTESIAN_POINT('Ctrl Pts',(7.09304587804797,-0.084143873775297,
-0.146299902363272));
#13266=CARTESIAN_POINT('Ctrl Pts',(7.16048806455421,0.209607112777233,-0.161999915098498));
#13267=CARTESIAN_POINT('Ctrl Pts',(7.44270302591942,0.315400242884882,-0.177699927833723));
#13268=CARTESIAN_POINT('Ctrl Pts',(7.68662571251122,0.138371518285505,-0.193399940568948));
#13269=CARTESIAN_POINT('Ctrl Pts',(7.67352840354824,-0.162736556273655,
-0.209099953304174));
#13270=CARTESIAN_POINT('Ctrl Pts',(7.41515553583245,-0.317917059776419,
-0.224799966039399));
#13271=CARTESIAN_POINT('Ctrl Pts',(7.14319256126489,-0.188018355137328,
-0.240499978774624));
#13272=CARTESIAN_POINT('Ctrl Pts',(7.10151127697963,0.110478246684683,-0.25619999150985));
#13273=CARTESIAN_POINT('Ctrl Pts',(7.32748769604729,0.309907927787576,-0.271900004245075));
#13274=CARTESIAN_POINT('Ctrl Pts',(7.61848659280405,0.231440205367399,-0.2876000169803));
#13275=CARTESIAN_POINT('Ctrl Pts',(7.71356646618244,-0.0545621737297924,
-0.303300029715526));
#13276=CARTESIAN_POINT('Ctrl Pts',(7.52746828088937,-0.291638126121681,
-0.319000042450751));
#13277=CARTESIAN_POINT('Ctrl Pts',(7.2270680653589,-0.267199374000224,-0.334700055185976));
#13278=CARTESIAN_POINT('Ctrl Pts',(7.08173757460019,-0.0031603793071512,
-0.350400067921202));
#13279=CARTESIAN_POINT('Ctrl Pts',(7.22179605399517,0.263712557575601,-0.366100080656427));
#13280=CARTESIAN_POINT('Ctrl Pts',(7.52165172137279,0.294111914264847,-0.381800093391652));
#13281=CARTESIAN_POINT('Ctrl Pts',(7.71242112312342,0.060778295782922,-0.397500106126878));
#13282=CARTESIAN_POINT('Ctrl Pts',(7.62303950654344,-0.227055803565647,
-0.413200118862103));
#13283=CARTESIAN_POINT('Ctrl Pts',(7.33365622468325,-0.311286785620935,
-0.428900131597329));
#13284=CARTESIAN_POINT('Ctrl Pts',(7.10376404266291,-0.116383920604752,
-0.444600144332554));
#13285=CARTESIAN_POINT('Ctrl Pts',(7.13950948546398,0.182881522455109,-0.460300157067779));
#13286=CARTESIAN_POINT('Ctrl Pts',(7.40883927184805,0.31815535003834,-0.476000169803005));
#13287=CARTESIAN_POINT('Ctrl Pts',(7.67024279803129,0.168136222607972,-0.49170018253823));
#13288=CARTESIAN_POINT('Ctrl Pts',(7.68931701530281,-0.132652267875577,
-0.507400195273454));
#13289=CARTESIAN_POINT('Ctrl Pts',(7.44895788800903,-0.314490198730143,
-0.523100208008681));
#13290=CARTESIAN_POINT('Ctrl Pts',(7.1646977556032,-0.214321748107725,-0.538800220743906));
#13291=CARTESIAN_POINT('Ctrl Pts',(7.09143539759574,0.0780310637115318,
-0.554500233479131));
#13292=CARTESIAN_POINT('Ctrl Pts',(7.29486588997329,0.300412685096896,-0.570200246214357));
#13293=CARTESIAN_POINT('Ctrl Pts',(7.5925711248828,0.253411343520026,-0.585900258949582));
#13294=CARTESIAN_POINT('Ctrl Pts',(7.71759603013189,-0.0208263280470064,
-0.601600271684807));
#13295=CARTESIAN_POINT('Ctrl Pts',(7.55782943657383,-0.276388938085432,
-0.617300284420033));
#13296=CARTESIAN_POINT('Ctrl Pts',(7.25653585808158,-0.28411072070256,-0.633000297155258));
#13297=CARTESIAN_POINT('Ctrl Pts',(7.08388757883703,-0.0370681282812828,
-0.648700309890483));
#13298=CARTESIAN_POINT('Ctrl Pts',(7.19470109296709,0.243214685511279,-0.664400322625709));
#13299=CARTESIAN_POINT('Ctrl Pts',(7.48960658835547,0.305402792280665,-0.680100335360934));
#13300=CARTESIAN_POINT('Ctrl Pts',(7.70416405875568,0.0937368459796346,
-0.695800348096159));
#13301=CARTESIAN_POINT('Ctrl Pts',(7.64596852236574,-0.201991011661366,
-0.711500360831385));
#13302=CARTESIAN_POINT('Ctrl Pts',(7.36722311255473,-0.316577103825418,
-0.727200373566609));
#13303=CARTESIAN_POINT('Ctrl Pts',(7.1178439182192,-0.147314693222106,-0.742900386301836));
#13304=CARTESIAN_POINT('Ctrl Pts',(7.12152748866831,0.154105168453245,-0.758600399037061));
#13305=CARTESIAN_POINT('Ctrl Pts',(7.37481774529794,0.317218457925703,-0.774300411772286));
#13306=CARTESIAN_POINT('Ctrl Pts',(7.65089575426731,0.196120165788626,-0.790000424507512));
#13307=CARTESIAN_POINT('Ctrl Pts',(7.70157185193576,-0.101340309887447,
-0.805700437242737));
#13308=CARTESIAN_POINT('Ctrl Pts',(7.55566596891409,-0.2381593775803,-0.816167112399554));
#13309=CARTESIAN_POINT('Ctrl Pts',(7.4698066426161,-0.261113218593862,-0.821400449977962));
#13310=CARTESIAN_POINT('Ctrl Pts',(7.61951971040191,0.187686343907875,0.0214004499779621));
#13311=CARTESIAN_POINT('Ctrl Pts',(7.68123478989901,0.115503807360182,0.0161671123995537));
#13312=CARTESIAN_POINT('Ctrl Pts',(7.72690688677709,-0.0932947832600543,
0.00570043724273678));
#13313=CARTESIAN_POINT('Ctrl Pts',(7.50223338226752,-0.3245682906377,-0.00999957549248855));
#13314=CARTESIAN_POINT('Ctrl Pts',(7.18581748555827,-0.264103571394519,
-0.0256995882277139));
#13315=CARTESIAN_POINT('Ctrl Pts',(7.06149699735691,0.0328478631389564,
-0.0413996009629392));
#13316=CARTESIAN_POINT('Ctrl Pts',(7.24069734678476,0.300510998934463,-0.0570996136981646));
#13317=CARTESIAN_POINT('Ctrl Pts',(7.56275487719186,0.298620437478645,-0.0727996264333898));
#13318=CARTESIAN_POINT('Ctrl Pts',(7.73886410297448,0.0289950124156803,
-0.0884996391686154));
#13319=CARTESIAN_POINT('Ctrl Pts',(7.61111284034442,-0.266650818298083,
-0.104199651903841));
#13320=CARTESIAN_POINT('Ctrl Pts',(7.29405357597622,-0.323178238317556,
-0.119899664639066));
#13321=CARTESIAN_POINT('Ctrl Pts',(7.07199802803806,-0.0899136208085419,
-0.135599677374291));
#13322=CARTESIAN_POINT('Ctrl Pts',(7.14406472656225,0.223979876507163,-0.151299690109517));
#13323=CARTESIAN_POINT('Ctrl Pts',(7.44563117322301,0.337027243568608,-0.166999702844742));
#13324=CARTESIAN_POINT('Ctrl Pts',(7.70627964309719,0.147859655939416,-0.182699715579967));
#13325=CARTESIAN_POINT('Ctrl Pts',(7.69228425140824,-0.173895405048169,
-0.198399728315193));
#13326=CARTESIAN_POINT('Ctrl Pts',(7.41619475121419,-0.339716638642509,
-0.214099741050418));
#13327=CARTESIAN_POINT('Ctrl Pts',(7.12558327028176,-0.200910777343205,
-0.229799753785644));
#13328=CARTESIAN_POINT('Ctrl Pts',(7.08104389953629,0.118053742171726,-0.245499766520869));
#13329=CARTESIAN_POINT('Ctrl Pts',(7.32251552597912,0.33115832032009,-0.261199779256094));
#13330=CARTESIAN_POINT('Ctrl Pts',(7.63346822264916,0.247310064673594,-0.276899791991319));
#13331=CARTESIAN_POINT('Ctrl Pts',(7.73506772476262,-0.0583035030254407,
-0.292599804726545));
#13332=CARTESIAN_POINT('Ctrl Pts',(7.53620878334662,-0.311635758004724,
-0.30829981746177));
#13333=CARTESIAN_POINT('Ctrl Pts',(7.21521011929483,-0.285521240183133,
-0.323999830196995));
#13334=CARTESIAN_POINT('Ctrl Pts',(7.05991431400671,-0.00337708657665555,
-0.339699842932221));
#13335=CARTESIAN_POINT('Ctrl Pts',(7.20957660601111,0.281795332689621,-0.355399855667446));
#13336=CARTESIAN_POINT('Ctrl Pts',(7.52999338223278,0.314279173848155,-0.371099868402671));
#13337=CARTESIAN_POINT('Ctrl Pts',(7.73384384550816,0.0649458646865791,
-0.386799881137897));
#13338=CARTESIAN_POINT('Ctrl Pts',(7.63833332977069,-0.242625024356483,
-0.402499893873122));
#13339=CARTESIAN_POINT('Ctrl Pts',(7.32910703074157,-0.332631726461441,
-0.418199906608347));
#13340=CARTESIAN_POINT('Ctrl Pts',(7.08345113740554,-0.124364368265385,
-0.433899919343573));
#13341=CARTESIAN_POINT('Ctrl Pts',(7.12164764590278,0.195421711945772,-0.449599932078798));
#13342=CARTESIAN_POINT('Ctrl Pts',(7.40944538088764,0.339971268472245,-0.465299944814024));
#13343=CARTESIAN_POINT('Ctrl Pts',(7.68877335185819,0.17966532660625,-0.480999957549249));
#13344=CARTESIAN_POINT('Ctrl Pts',(7.70915548857264,-0.141748236419551,
-0.496699970284474));
#13345=CARTESIAN_POINT('Ctrl Pts',(7.45231493132566,-0.336054797668783,
-0.5123999830197));
#13346=CARTESIAN_POINT('Ctrl Pts',(7.14856307620694,-0.229017794472391,
-0.528099995754925));
#13347=CARTESIAN_POINT('Ctrl Pts',(7.07027711691044,0.0833816552418533,
-0.543800008490151));
#13348=CARTESIAN_POINT('Ctrl Pts',(7.28765684203904,0.321011988656602,-0.559500021225375));
#13349=CARTESIAN_POINT('Ctrl Pts',(7.60577573059716,0.27078776418934,-0.575200033960601));
#13350=CARTESIAN_POINT('Ctrl Pts',(7.73937359598911,-0.0222543897593003,
-0.590900046695826));
#13351=CARTESIAN_POINT('Ctrl Pts',(7.56865180405673,-0.29534093285333,-0.606600059431052));
#13352=CARTESIAN_POINT('Ctrl Pts',(7.24669851912781,-0.303592198252122,
-0.622300072166277));
#13353=CARTESIAN_POINT('Ctrl Pts',(7.06221174407517,-0.0396098905461152,
-0.638000084901503));
#13354=CARTESIAN_POINT('Ctrl Pts',(7.1806237429874,0.259891921146016,-0.653700097636727));
#13355=CARTESIAN_POINT('Ctrl Pts',(7.4957509138319,0.326344267585352,-0.669400110371953));
#13356=CARTESIAN_POINT('Ctrl Pts',(7.72502059407888,0.100164383300307,-0.685100123107178));
#13357=CARTESIAN_POINT('Ctrl Pts',(7.66283458864623,-0.215841539192194,
-0.700800135842403));
#13358=CARTESIAN_POINT('Ctrl Pts',(7.36497560075606,-0.338284801886334,
-0.71650014857763));
#13359=CARTESIAN_POINT('Ctrl Pts',(7.09849647029787,-0.157416064552375,
-0.732200161312854));
#13360=CARTESIAN_POINT('Ctrl Pts',(7.10243262324309,0.164672162799918,-0.74790017404808));
#13361=CARTESIAN_POINT('Ctrl Pts',(7.37309099761164,0.338970133649535,-0.763600186783305));
#13362=CARTESIAN_POINT('Ctrl Pts',(7.66809968093348,0.209568129305734,-0.77930019951853));
#13363=CARTESIAN_POINT('Ctrl Pts',(7.72225063958776,-0.108289216873624,
-0.795000212253756));
#13364=CARTESIAN_POINT('Ctrl Pts',(7.5663399873782,-0.254489970653575,-0.805466887410573));
#13365=CARTESIAN_POINT('Ctrl Pts',(7.47459328543469,-0.279017756984216,
-0.810700224988981));
#13366=CARTESIAN_POINT('Ctrl Pts',(7.63360626576962,0.199730155693065,0.0321006749669432));
#13367=CARTESIAN_POINT('Ctrl Pts',(7.69928159504458,0.122915673814364,0.0268673373885347));
#13368=CARTESIAN_POINT('Ctrl Pts',(7.74788446529264,-0.0992814991112389,
0.0164006622317179));
#13369=CARTESIAN_POINT('Ctrl Pts',(7.50879368702149,-0.345395801699454,
0.000700649496492501));
#13370=CARTESIAN_POINT('Ctrl Pts',(7.17207341746091,-0.281051068156635,
-0.0149993632387328));
#13371=CARTESIAN_POINT('Ctrl Pts',(7.03977529737773,0.0349557068581856,
-0.0306993759739581));
#13372=CARTESIAN_POINT('Ctrl Pts',(7.23047491327011,0.319794756266977,-0.0463993887091836));
#13373=CARTESIAN_POINT('Ctrl Pts',(7.5731988395346,0.317782877693097,-0.0620994014444088));
#13374=CARTESIAN_POINT('Ctrl Pts',(7.76060897472171,0.0308556191331042,
-0.0777994141796343));
#13375=CARTESIAN_POINT('Ctrl Pts',(7.62465992779684,-0.283761771610304,
-0.0934994269148594));
#13376=CARTESIAN_POINT('Ctrl Pts',(7.2872550057463,-0.343916549876741,-0.109199439650085));
#13377=CARTESIAN_POINT('Ctrl Pts',(7.05095017802815,-0.0956833678417867,
-0.12489945238531));
#13378=CARTESIAN_POINT('Ctrl Pts',(7.12764138857029,0.238352640237094,-0.140599465120536));
#13379=CARTESIAN_POINT('Ctrl Pts',(7.4485593205266,0.358654244252335,-0.156299477855761));
#13380=CARTESIAN_POINT('Ctrl Pts',(7.72593357368315,0.157347793593328,-0.171999490590986));
#13381=CARTESIAN_POINT('Ctrl Pts',(7.71104009926825,-0.185054253822684,
-0.187699503326212));
#13382=CARTESIAN_POINT('Ctrl Pts',(7.41723396659593,-0.361516217508599,
-0.203399516061437));
#13383=CARTESIAN_POINT('Ctrl Pts',(7.10797397929862,-0.213803199549082,
-0.219099528796662));
#13384=CARTESIAN_POINT('Ctrl Pts',(7.06057652209295,0.125629237658768,-0.234799541531888));
#13385=CARTESIAN_POINT('Ctrl Pts',(7.31754335591095,0.352408712852604,-0.250499554267113));
#13386=CARTESIAN_POINT('Ctrl Pts',(7.64844985249427,0.263179923979787,-0.266199567002338));
#13387=CARTESIAN_POINT('Ctrl Pts',(7.75656898334281,-0.062044832321089,
-0.281899579737564));
#13388=CARTESIAN_POINT('Ctrl Pts',(7.54494928580385,-0.331633389887768,
-0.297599592472789));
#13389=CARTESIAN_POINT('Ctrl Pts',(7.20335217323078,-0.303843106366043,
-0.313299605208014));
#13390=CARTESIAN_POINT('Ctrl Pts',(7.03809105341322,-0.00359379384616002,
-0.32899961794324));
#13391=CARTESIAN_POINT('Ctrl Pts',(7.19735715802706,0.299878107803642,-0.344699630678465));
#13392=CARTESIAN_POINT('Ctrl Pts',(7.53833504309277,0.334446433431464,-0.36039964341369));
#13393=CARTESIAN_POINT('Ctrl Pts',(7.75526656789289,0.0691134335902364,
-0.376099656148916));
#13394=CARTESIAN_POINT('Ctrl Pts',(7.65362715299794,-0.25819424514732,-0.391799668884141));
#13395=CARTESIAN_POINT('Ctrl Pts',(7.32455783679988,-0.353976667301946,
-0.407499681619366));
#13396=CARTESIAN_POINT('Ctrl Pts',(7.06313823214816,-0.132344815926019,
-0.423199694354592));
#13397=CARTESIAN_POINT('Ctrl Pts',(7.10378580634158,0.207961901436435,-0.438899707089817));
#13398=CARTESIAN_POINT('Ctrl Pts',(7.41005148992723,0.36178718690615,-0.454599719825043));
#13399=CARTESIAN_POINT('Ctrl Pts',(7.70730390568508,0.191194430604527,-0.470299732560268));
#13400=CARTESIAN_POINT('Ctrl Pts',(7.72899396184246,-0.150844204963527,
-0.485999745295493));
#13401=CARTESIAN_POINT('Ctrl Pts',(7.45567197464232,-0.357619396607422,
-0.501699758030719));
#13402=CARTESIAN_POINT('Ctrl Pts',(7.13242839681067,-0.243713840837058,
-0.517399770765943));
#13403=CARTESIAN_POINT('Ctrl Pts',(7.04911883622514,0.088732246772175,-0.533099783501169));
#13404=CARTESIAN_POINT('Ctrl Pts',(7.28044779410479,0.341611292216308,-0.548799796236394));
#13405=CARTESIAN_POINT('Ctrl Pts',(7.61898033631151,0.288164184858654,-0.564499808971621));
#13406=CARTESIAN_POINT('Ctrl Pts',(7.76115116184634,-0.0236824514715945,
-0.580199821706845));
#13407=CARTESIAN_POINT('Ctrl Pts',(7.57947417153963,-0.314292927621228,
-0.595899834442071));
#13408=CARTESIAN_POINT('Ctrl Pts',(7.23686118017403,-0.323073675801685,
-0.611599847177295));
#13409=CARTESIAN_POINT('Ctrl Pts',(7.0405359093133,-0.0421516528109474,
-0.627299859912522));
#13410=CARTESIAN_POINT('Ctrl Pts',(7.16654639300772,0.276569156780754,-0.642999872647746));
#13411=CARTESIAN_POINT('Ctrl Pts',(7.50189523930833,0.347285742890038,-0.658699885382972));
#13412=CARTESIAN_POINT('Ctrl Pts',(7.74587712940208,0.10659192062098,-0.674399898118197));
#13413=CARTESIAN_POINT('Ctrl Pts',(7.67970065492672,-0.229692066723022,
-0.690099910853423));
#13414=CARTESIAN_POINT('Ctrl Pts',(7.36272808895739,-0.359992499947249,
-0.705799923588647));
#13415=CARTESIAN_POINT('Ctrl Pts',(7.07914902237653,-0.167517435882645,
-0.721499936323874));
#13416=CARTESIAN_POINT('Ctrl Pts',(7.08333775781787,0.175239157146592,-0.737199949059098));
#13417=CARTESIAN_POINT('Ctrl Pts',(7.37136424992534,0.360721809373367,-0.752899961794324));
#13418=CARTESIAN_POINT('Ctrl Pts',(7.68530360759964,0.223016092822843,-0.768599974529549));
#13419=CARTESIAN_POINT('Ctrl Pts',(7.74292942723977,-0.115238123859802,
-0.784299987264775));
#13420=CARTESIAN_POINT('Ctrl Pts',(7.57701400584231,-0.270820563726849,
-0.794766662421592));
#13421=CARTESIAN_POINT('Ctrl Pts',(7.47937992825329,-0.29692229537457,-0.8));
#13422=CARTESIAN_POINT('Ctrl Pts',(7.59134659966651,0.163598720337495,0.));
#13423=CARTESIAN_POINT('Ctrl Pts',(7.60250981747379,0.153108036753198,-2.76372047324665E-18));
#13424=CARTESIAN_POINT('Ctrl Pts',(7.61257002986606,0.141586745509806,-2.10635142953706E-17));
#13425=CARTESIAN_POINT('Ctrl Pts',(7.62152230270038,0.129252348737935,-1.17093834628434E-17));
#13426=CARTESIAN_POINT('Ctrl Pts',(7.62952885125357,0.118220966154305,-3.34342946773069E-18));
#13427=CARTESIAN_POINT('Ctrl Pts',(7.63664920495495,0.106537870238012,-2.15761777783297E-17));
#13428=CARTESIAN_POINT('Ctrl Pts',(7.64286041237134,0.0943311530405987,
-2.77555756156289E-17));
#13429=CARTESIAN_POINT('Ctrl Pts',(7.64494079815862,0.0902426273700751,
-2.98253070821307E-17));
#13430=CARTESIAN_POINT('Ctrl Pts',(7.64691967101295,0.0860937108205726,
2.22114370828616E-17));
#13431=CARTESIAN_POINT('Ctrl Pts',(7.64879354491767,0.081893408177734,1.64798730217797E-17));
#13432=CARTESIAN_POINT('Ctrl Pts',(7.655493762727,0.0668748188792052,-4.01388992607871E-18));
#13433=CARTESIAN_POINT('Ctrl Pts',(7.6608110935522,0.0513021332299394,3.07095711685637E-17));
#13434=CARTESIAN_POINT('Ctrl Pts',(7.66472282738542,0.0354014324049846,
3.46944695195361E-17));
#13435=CARTESIAN_POINT('Ctrl Pts',(7.66742756504633,0.0244070176033393,
3.74497962120694E-17));
#13436=CARTESIAN_POINT('Ctrl Pts',(7.66945962470024,0.0132547133788681,
7.12360322228779E-17));
#13437=CARTESIAN_POINT('Ctrl Pts',(7.67079967407203,0.00201093560136876,
9.19403442267708E-17));
#13438=CARTESIAN_POINT('Ctrl Pts',(7.67155462684706,-0.00432354834646305,
1.03604674012976E-16));
#13439=CARTESIAN_POINT('Ctrl Pts',(7.67208975223811,-0.0106871591093033,
5.10024386813213E-17));
#13440=CARTESIAN_POINT('Ctrl Pts',(7.67239999929748,-0.017068447894435,
6.07153216591882E-17));
#13441=CARTESIAN_POINT('Ctrl Pts',(7.67261026346053,-0.0213932474537081,
6.72980470985737E-17));
#13442=CARTESIAN_POINT('Ctrl Pts',(7.67271673802996,-0.0257170992981115,
4.2195820725283E-17));
#13443=CARTESIAN_POINT('Ctrl Pts',(7.67271892939023,-0.0300345419010102,
4.33680868994202E-17));
#13444=CARTESIAN_POINT('Ctrl Pts',(7.67272693146828,-0.0458003258944295,
4.76487912385652E-17));
#13445=CARTESIAN_POINT('Ctrl Pts',(7.67134758489843,-0.0614867913330191,
6.01689604624523E-17));
#13446=CARTESIAN_POINT('Ctrl Pts',(7.66853812911313,-0.0769181334380825,
6.93889390390723E-17));
#13447=CARTESIAN_POINT('Ctrl Pts',(7.6662196457605,-0.0896527384696332,
7.30753135663338E-17));
#13448=CARTESIAN_POINT('Ctrl Pts',(7.66292674408646,-0.102214296971847,
6.38087454160287E-17));
#13449=CARTESIAN_POINT('Ctrl Pts',(7.65873262674493,-0.114535513997406,
6.24500451351651E-17));
#13450=CARTESIAN_POINT('Ctrl Pts',(7.65678779272614,-0.120248926396956,
6.18200087502971E-17));
#13451=CARTESIAN_POINT('Ctrl Pts',(7.65464687544019,-0.125914602381379,
5.65864599207131E-17));
#13452=CARTESIAN_POINT('Ctrl Pts',(7.65232789334325,-0.131499045448586,
5.89805981832114E-17));
#13453=CARTESIAN_POINT('Ctrl Pts',(7.64581346085479,-0.147186737645481,
6.57061576860812E-17));
#13454=CARTESIAN_POINT('Ctrl Pts',(7.63788690776836,-0.162272369755971,
2.69522798546906E-17));
#13455=CARTESIAN_POINT('Ctrl Pts',(7.62872587899731,-0.176613455703731,
2.08166817117217E-17));
#13456=CARTESIAN_POINT('Ctrl Pts',(7.62337452143084,-0.184990711219019,
1.7232610493544E-17));
#13457=CARTESIAN_POINT('Ctrl Pts',(7.61760089383393,-0.193113914513073,
7.21698909598366E-17));
#13458=CARTESIAN_POINT('Ctrl Pts',(7.61143279113021,-0.200952905400778,
8.32667268468867E-17));
#13459=CARTESIAN_POINT('Ctrl Pts',(7.60742014858138,-0.20605253974327,9.04857434516068E-17));
#13460=CARTESIAN_POINT('Ctrl Pts',(7.60324045059445,-0.211031857377795,
2.3759156340358E-17));
#13461=CARTESIAN_POINT('Ctrl Pts',(7.59890027835381,-0.215881931042746,
1.73472347597681E-17));
#13462=CARTESIAN_POINT('Ctrl Pts',(7.59567072863155,-0.219490901652473,
1.25760831990297E-17));
#13463=CARTESIAN_POINT('Ctrl Pts',(7.59235503385033,-0.22302506289888,3.58617524316929E-17));
#13464=CARTESIAN_POINT('Ctrl Pts',(7.58896204714281,-0.226475380907007,
3.81639164714898E-17));
#13465=CARTESIAN_POINT('Ctrl Pts',(7.57975197943177,-0.235841071143565,
4.44130086478315E-17));
#13466=CARTESIAN_POINT('Ctrl Pts',(7.56996175646191,-0.244602587321019,
6.41428917201894E-17));
#13467=CARTESIAN_POINT('Ctrl Pts',(7.5596547346654,-0.252692752680651,5.89805981832114E-17));
#13468=CARTESIAN_POINT('Ctrl Pts',(7.55492270000885,-0.256407011136178,
5.66105486765211E-17));
#13469=CARTESIAN_POINT('Ctrl Pts',(7.55008155466001,-0.259979662792626,
6.18911852966909E-17));
#13470=CARTESIAN_POINT('Ctrl Pts',(7.5451366005002,-0.263403568695713,5.89805981832114E-17));
#13471=CARTESIAN_POINT('Ctrl Pts',(7.53997605228505,-0.266976752779113,
5.59431129714072E-17));
#13472=CARTESIAN_POINT('Ctrl Pts',(7.53470889794899,-0.270383320907462,
7.04757199048251E-17));
#13473=CARTESIAN_POINT('Ctrl Pts',(7.5293467893667,-0.273613072908771,6.59194920871187E-17));
#13474=CARTESIAN_POINT('Ctrl Pts',(7.51740496593982,-0.280805976133378,
5.57724263840117E-17));
#13475=CARTESIAN_POINT('Ctrl Pts',(7.50498570886338,-0.287127913581425,
1.04560758728475E-17));
#13476=CARTESIAN_POINT('Ctrl Pts',(7.4921567849037,-0.292493152066132,-6.93889390390723E-18));
#13477=CARTESIAN_POINT('Ctrl Pts',(7.48800667626404,-0.294228786532378,
-5.43963370827884E-18));
#13478=CARTESIAN_POINT('Ctrl Pts',(7.48381360175906,-0.295864191924157,
9.75249754612042E-18));
#13479=CARTESIAN_POINT('Ctrl Pts',(7.47958090815733,-0.297400289619931,
6.93889390390723E-18));
#13480=CARTESIAN_POINT('Ctrl Pts',(7.1483354802531,-0.000213511019231185,
-0.161258330249198));
#13481=CARTESIAN_POINT('Ctrl Pts',(7.14814623960277,-0.0226803112827391,
-0.15983892928355));
#13482=CARTESIAN_POINT('Ctrl Pts',(7.15091292268037,-0.0451013034050039,
-0.158419528317902));
#13483=CARTESIAN_POINT('Ctrl Pts',(7.15682283853563,-0.0666606288533484,
-0.157000127352254));
#13484=CARTESIAN_POINT('Ctrl Pts',(7.17861272418395,-0.146149956227763,
-0.151766789773846));
#13485=CARTESIAN_POINT('Ctrl Pts',(7.24313172031002,-0.213925785713474,
-0.146533452195437));
#13486=CARTESIAN_POINT('Ctrl Pts',(7.32145254320697,-0.239601583202072,
-0.141300114617029));
#13487=CARTESIAN_POINT('Ctrl Pts',(7.39977336610391,-0.26527738069067,-0.13606677703862));
#13488=CARTESIAN_POINT('Ctrl Pts',(7.49189601577174,-0.248853146182156,
-0.130833439460212));
#13489=CARTESIAN_POINT('Ctrl Pts',(7.55651662294573,-0.197690577152153,
-0.125600101881803));
#13490=CARTESIAN_POINT('Ctrl Pts',(7.62113723011973,-0.14652800812215,-0.120366764303395));
#13491=CARTESIAN_POINT('Ctrl Pts',(7.65825579479988,-0.0606271045706585,
-0.115133426724986));
#13492=CARTESIAN_POINT('Ctrl Pts',(7.65123050931102,0.0214936402165713,
-0.109900089146578));
#13493=CARTESIAN_POINT('Ctrl Pts',(7.64420522382215,0.103614385003801,-0.104666751568169));
#13494=CARTESIAN_POINT('Ctrl Pts',(7.59303608816426,0.18195497102677,-0.099433413989761));
#13495=CARTESIAN_POINT('Ctrl Pts',(7.5206640638866,0.22139991857487,-0.0942000764113525));
#13496=CARTESIAN_POINT('Ctrl Pts',(7.44829203960894,0.260844866122971,-0.0889667388329441));
#13497=CARTESIAN_POINT('Ctrl Pts',(7.3547171267115,0.261394175196203,-0.0837334012545357));
#13498=CARTESIAN_POINT('Ctrl Pts',(7.28189603417964,0.222783611637997,-0.0785000636761272));
#13499=CARTESIAN_POINT('Ctrl Pts',(7.20907494164779,0.18417304807979,-0.0732667260977188));
#13500=CARTESIAN_POINT('Ctrl Pts',(7.15700766948152,0.106402611890144,-0.0680333885193103));
#13501=CARTESIAN_POINT('Ctrl Pts',(7.14903490413801,0.0243772682001904,
-0.0628000509409019));
#13502=CARTESIAN_POINT('Ctrl Pts',(7.14825198902148,0.0163224868606074,
-0.0622861440436673));
#13503=CARTESIAN_POINT('Ctrl Pts',(7.14789427647666,0.00822667552110126,
-0.0617722371464327));
#13504=CARTESIAN_POINT('Ctrl Pts',(7.14794643808389,0.00012639595204536,
-0.0612583302491982));
#13505=CARTESIAN_POINT('Ctrl Pts',(7.32062007174671,-0.29692229537457,0.));
#13506=CARTESIAN_POINT('Ctrl Pts',(7.22298599415769,-0.270820563726849,
-0.00523333757840845));
#13507=CARTESIAN_POINT('Ctrl Pts',(7.05707055753998,-0.115238222676569,
-0.0157000127352254));
#13508=CARTESIAN_POINT('Ctrl Pts',(7.11469640556356,0.223016129191749,-0.0314000254704506));
#13509=CARTESIAN_POINT('Ctrl Pts',(7.42863574892529,0.360721777030891,-0.047100038205676));
#13510=CARTESIAN_POINT('Ctrl Pts',(7.71666223333994,0.175239166203998,-0.0628000509409013));
#13511=CARTESIAN_POINT('Ctrl Pts',(7.72085097116846,-0.167517439243982,
-0.0785000636761268));
#13512=CARTESIAN_POINT('Ctrl Pts',(7.43727190914667,-0.359992487166362,
-0.094200076411352));
#13513=CARTESIAN_POINT('Ctrl Pts',(7.12029935249992,-0.229692063399103,
-0.109900089146577));
#13514=CARTESIAN_POINT('Ctrl Pts',(7.05412287853826,0.106591919249608,-0.125600101881803));
#13515=CARTESIAN_POINT('Ctrl Pts',(7.2981047634038,0.347285733851148,-0.141300114617028));
#13516=CARTESIAN_POINT('Ctrl Pts',(7.63345360120587,0.276569150443068,-0.157000127352253));
#13517=CARTESIAN_POINT('Ctrl Pts',(7.75946408208296,-0.0421516519758924,
-0.172700140087479));
#13518=CARTESIAN_POINT('Ctrl Pts',(7.56313881583769,-0.323073667897745,
-0.188400152822704));
#13519=CARTESIAN_POINT('Ctrl Pts',(7.22052583282271,-0.314292920077652,
-0.20410016555793));
#13520=CARTESIAN_POINT('Ctrl Pts',(7.03884884686676,-0.023682450872479,
-0.219800178293155));
#13521=CARTESIAN_POINT('Ctrl Pts',(7.18101966898755,0.28816417788129,-0.23550019102838));
#13522=CARTESIAN_POINT('Ctrl Pts',(7.51955220300225,0.341611283968803,-0.251200203763605));
#13523=CARTESIAN_POINT('Ctrl Pts',(7.7508811552982,0.0887322446241938,-0.266900216498831));
#13524=CARTESIAN_POINT('Ctrl Pts',(7.66757159672246,-0.243713834945875,
-0.282600229234056));
#13525=CARTESIAN_POINT('Ctrl Pts',(7.34432802670357,-0.357619387966788,
-0.298300241969282));
#13526=CARTESIAN_POINT('Ctrl Pts',(7.07100604610717,-0.150844201317933,
-0.314000254704507));
#13527=CARTESIAN_POINT('Ctrl Pts',(7.0926961017409,0.191194425984153,-0.329700267439732));
#13528=CARTESIAN_POINT('Ctrl Pts',(7.38994851031558,0.361787178163918,-0.345400280174957));
#13529=CARTESIAN_POINT('Ctrl Pts',(7.69621418650062,0.207961896411083,-0.361100292910183));
#13530=CARTESIAN_POINT('Ctrl Pts',(7.73686175971175,-0.132344812727946,
-0.376800305645408));
#13531=CARTESIAN_POINT('Ctrl Pts',(7.47544216137711,-0.353976658748332,
-0.392500318380634));
#13532=CARTESIAN_POINT('Ctrl Pts',(7.14637285313081,-0.258194238908191,
-0.408200331115859));
#13533=CARTESIAN_POINT('Ctrl Pts',(7.04473344069191,0.0691134319201361,
-0.423900343851084));
#13534=CARTESIAN_POINT('Ctrl Pts',(7.26166496025002,0.334446425349789,-0.43960035658631));
#13535=CARTESIAN_POINT('Ctrl Pts',(7.60264283707619,0.299878100557217,-0.455300369321535));
#13536=CARTESIAN_POINT('Ctrl Pts',(7.76190893784147,-0.00359379375923244,
-0.47100038205676));
#13537=CARTESIAN_POINT('Ctrl Pts',(7.59664782201734,-0.303843099024022,
-0.486700394791986));
#13538=CARTESIAN_POINT('Ctrl Pts',(7.25505071769875,-0.33163338187372,-0.502400407527211));
#13539=CARTESIAN_POINT('Ctrl Pts',(7.0434310252735,-0.0620448308224301,
-0.518100420262436));
#13540=CARTESIAN_POINT('Ctrl Pts',(7.1515501535093,0.263179917621393,-0.533800432997662));
#13541=CARTESIAN_POINT('Ctrl Pts',(7.4824566420967,0.352408704334569,-0.549500445732887));
#13542=CARTESIAN_POINT('Ctrl Pts',(7.73942346970471,0.125629234627381,-0.565200458468113));
#13543=CARTESIAN_POINT('Ctrl Pts',(7.69202601364555,-0.213803194390989,
-0.580900471203338));
#13544=CARTESIAN_POINT('Ctrl Pts',(7.38276603381877,-0.361516208756931,
-0.596600483938563));
#13545=CARTESIAN_POINT('Ctrl Pts',(7.08895990825159,-0.185054249380952,
-0.612300496673788));
#13546=CARTESIAN_POINT('Ctrl Pts',(7.07406643418487,0.157347789847665,-0.628000509409014));
#13547=CARTESIAN_POINT('Ctrl Pts',(7.35144068066377,0.358654235479558,-0.643700522144239));
#13548=CARTESIAN_POINT('Ctrl Pts',(7.67235860481237,0.238352634675404,-0.659400534879465));
#13549=CARTESIAN_POINT('Ctrl Pts',(7.74904981361332,-0.0956833658965494,
-0.675100547614689));
#13550=CARTESIAN_POINT('Ctrl Pts',(7.51274499136877,-0.343916540891515,
-0.690800560349916));
#13551=CARTESIAN_POINT('Ctrl Pts',(7.17534007797001,-0.283761765982407,
-0.70650057308514));
#13552=CARTESIAN_POINT('Ctrl Pts',(7.03939103328141,0.0308556206006142,
-0.722200585820366));
#13553=CARTESIAN_POINT('Ctrl Pts',(7.22680116614257,0.317782866086405,-0.737900598555591));
#13554=CARTESIAN_POINT('Ctrl Pts',(7.56952507950631,0.319794755380677,-0.753600611290817));
#13555=CARTESIAN_POINT('Ctrl Pts',(7.76022470046591,0.0349556943853752,
-0.769300624026041));
#13556=CARTESIAN_POINT('Ctrl Pts',(7.62792656327177,-0.28105104215419,-0.785000636761267));
#13557=CARTESIAN_POINT('Ctrl Pts',(7.29120634442719,-0.345395824214954,
-0.800700649496492));
#13558=CARTESIAN_POINT('Ctrl Pts',(7.0521154661904,-0.099281426297527,-0.816400662231718));
#13559=CARTESIAN_POINT('Ctrl Pts',(7.10071840495542,0.122915673814367,-0.826867337388535));
#13560=CARTESIAN_POINT('Ctrl Pts',(7.16639373423039,0.199730155693067,-0.832100674966943));
#13561=CARTESIAN_POINT('Ctrl Pts',(7.32540671456531,-0.279017756984216,
0.0107002249889811));
#13562=CARTESIAN_POINT('Ctrl Pts',(7.2336600126218,-0.254489970653575,0.00546688741057261));
#13563=CARTESIAN_POINT('Ctrl Pts',(7.07774934610977,-0.108289309731699,
-0.00499978774624428));
#13564=CARTESIAN_POINT('Ctrl Pts',(7.13190033143599,0.20956816348158,-0.0206998004814696));
#13565=CARTESIAN_POINT('Ctrl Pts',(7.42690900130829,0.338970103257324,-0.036399813216695));
#13566=CARTESIAN_POINT('Ctrl Pts',(7.69756736844791,0.164672171311159,-0.0520998259519203));
#13567=CARTESIAN_POINT('Ctrl Pts',(7.70150352363636,-0.157416067711022,
-0.0677998386871457));
#13568=CARTESIAN_POINT('Ctrl Pts',(7.43502439746233,-0.338284789876139,
-0.0834998514223709));
#13569=CARTESIAN_POINT('Ctrl Pts',(7.13716541833258,-0.215841536068708,
-0.0991998641575964));
#13570=CARTESIAN_POINT('Ctrl Pts',(7.07497941338266,0.10016438201163,-0.114899876892821));
#13571=CARTESIAN_POINT('Ctrl Pts',(7.30424908871668,0.32634425909151,-0.130599889628047));
#13572=CARTESIAN_POINT('Ctrl Pts',(7.61937625157511,0.259891915190496,-0.146299902363272));
#13573=CARTESIAN_POINT('Ctrl Pts',(7.7377882478399,-0.0396098897614143,
-0.161999915098498));
#13574=CARTESIAN_POINT('Ctrl Pts',(7.5533014771244,-0.303592190824794,-0.177699927833723));
#13575=CARTESIAN_POINT('Ctrl Pts',(7.23134820004257,-0.295340925764635,
-0.193399940568948));
#13576=CARTESIAN_POINT('Ctrl Pts',(7.06062641219857,-0.022254389196312,
-0.209099953304174));
#13577=CARTESIAN_POINT('Ctrl Pts',(7.19422427438237,0.270787757632714,-0.224799966039399));
#13578=CARTESIAN_POINT('Ctrl Pts',(7.51234315524245,0.321011980906425,-0.240499978774625));
#13579=CARTESIAN_POINT('Ctrl Pts',(7.72972287512404,0.0833816532233965,
-0.25619999150985));
#13580=CARTESIAN_POINT('Ctrl Pts',(7.65143691771615,-0.22901778893645,-0.271900004245075));
#13581=CARTESIAN_POINT('Ctrl Pts',(7.34768506993906,-0.336054789549182,
-0.2876000169803));
#13582=CARTESIAN_POINT('Ctrl Pts',(7.09084451889762,-0.141748232993789,
-0.303300029715526));
#13583=CARTESIAN_POINT('Ctrl Pts',(7.11122665512001,0.179665322264485,-0.319000042450751));
#13584=CARTESIAN_POINT('Ctrl Pts',(7.39055461934053,0.339971260257174,-0.334700055185976));
#13585=CARTESIAN_POINT('Ctrl Pts',(7.67835234737104,0.195421707223451,-0.350400067921202));
#13586=CARTESIAN_POINT('Ctrl Pts',(7.71654885494523,-0.124364365260158,
-0.366100080656428));
#13587=CARTESIAN_POINT('Ctrl Pts',(7.47089296754535,-0.332631718423613,
-0.381800093391652));
#13588=CARTESIAN_POINT('Ctrl Pts',(7.16166667598849,-0.242625018493576,
-0.397500106126878));
#13589=CARTESIAN_POINT('Ctrl Pts',(7.06615616255898,0.0649458631171862,
-0.413200118862103));
#13590=CARTESIAN_POINT('Ctrl Pts',(7.27000662090844,0.314279166253809,-0.428900131597329));
#13591=CARTESIAN_POINT('Ctrl Pts',(7.59042338938741,0.281795325880159,-0.444600144332553));
#13592=CARTESIAN_POINT('Ctrl Pts',(7.74008567777533,-0.00337708649496984,
-0.46030015706778));
#13593=CARTESIAN_POINT('Ctrl Pts',(7.58478987623982,-0.285521233283839,
-0.476000169803004));
#13594=CARTESIAN_POINT('Ctrl Pts',(7.26379121994478,-0.311635750473927,
-0.491700182538231));
#13595=CARTESIAN_POINT('Ctrl Pts',(7.06493228333412,-0.0583035016171516,
-0.507400195273454));
#13596=CARTESIAN_POINT('Ctrl Pts',(7.16653178299239,0.247310058698613,-0.523100208008682));
#13597=CARTESIAN_POINT('Ctrl Pts',(7.47748447214868,0.331158312315696,-0.538800220743906));
#13598=CARTESIAN_POINT('Ctrl Pts',(7.71895609275597,0.118053739323133,-0.554500233479132));
#13599=CARTESIAN_POINT('Ctrl Pts',(7.67441672308789,-0.200910772496147,
-0.570200246214356));
#13600=CARTESIAN_POINT('Ctrl Pts',(7.3838052491755,-0.339716630418571,-0.585900258949582));
#13601=CARTESIAN_POINT('Ctrl Pts',(7.10771575565814,-0.173895400874276,
-0.601600271684807));
#13602=CARTESIAN_POINT('Ctrl Pts',(7.09372036429638,0.147859652419619,-0.617300284420033));
#13603=CARTESIAN_POINT('Ctrl Pts',(7.35436882789558,0.337027235324834,-0.633000297155258));
#13604=CARTESIAN_POINT('Ctrl Pts',(7.65593526721943,0.223979871280845,-0.648700309890484));
#13605=CARTESIAN_POINT('Ctrl Pts',(7.72800196410744,-0.0899136189806033,
-0.664400322625708));
#13606=CARTESIAN_POINT('Ctrl Pts',(7.5059464213128,-0.323178229874143,-0.680100335360935));
#13607=CARTESIAN_POINT('Ctrl Pts',(7.18888716507469,-0.266650813009551,
-0.695800348096159));
#13608=CARTESIAN_POINT('Ctrl Pts',(7.06113590454605,0.028995013794699,-0.711500360831385));
#13609=CARTESIAN_POINT('Ctrl Pts',(7.23724512814298,0.298620426571841,-0.72720037356661));
#13610=CARTESIAN_POINT('Ctrl Pts',(7.55930264642725,0.300510998101608,-0.742900386301836));
#13611=CARTESIAN_POINT('Ctrl Pts',(7.73850300061676,0.0328478514182617,
-0.758600399037061));
#13612=CARTESIAN_POINT('Ctrl Pts',(7.61418249633623,-0.264103546960032,
-0.774300411772286));
#13613=CARTESIAN_POINT('Ctrl Pts',(7.29776664728478,-0.324568311795507,
-0.790000424507512));
#13614=CARTESIAN_POINT('Ctrl Pts',(7.07309304883756,-0.0932947148370394,
-0.805700437242737));
#13615=CARTESIAN_POINT('Ctrl Pts',(7.118765210101,0.115503807360185,-0.816167112399554));
#13616=CARTESIAN_POINT('Ctrl Pts',(7.18048028959809,0.187686343907877,-0.821400449977962));
#13617=CARTESIAN_POINT('Ctrl Pts',(7.3301933573839,-0.261113218593861,0.0214004499779621));
#13618=CARTESIAN_POINT('Ctrl Pts',(7.24433403108591,-0.2381593775803,0.0161671123995537));
#13619=CARTESIAN_POINT('Ctrl Pts',(7.09842813467957,-0.10134039678683,0.00570043724273678));
#13620=CARTESIAN_POINT('Ctrl Pts',(7.1491042573084,0.196120197771411,-0.00999957549248853));
#13621=CARTESIAN_POINT('Ctrl Pts',(7.42518225369131,0.317218429483757,-0.0256995882277139));
#13622=CARTESIAN_POINT('Ctrl Pts',(7.67847250355587,0.154105176418319,-0.0413996009629392));
#13623=CARTESIAN_POINT('Ctrl Pts',(7.68215607610427,-0.147314696178063,
-0.0570996136981647));
#13624=CARTESIAN_POINT('Ctrl Pts',(7.43277688577798,-0.316577092585917,
-0.0727996264333898));
#13625=CARTESIAN_POINT('Ctrl Pts',(7.15403148416523,-0.201991008738314,
-0.0884996391686153));
#13626=CARTESIAN_POINT('Ctrl Pts',(7.09583594822706,0.093736844773651,-0.104199651903841));
#13627=CARTESIAN_POINT('Ctrl Pts',(7.31039341402957,0.305402784331873,-0.119899664639066));
#13628=CARTESIAN_POINT('Ctrl Pts',(7.60529890194435,0.243214679937923,-0.135599677374291));
#13629=CARTESIAN_POINT('Ctrl Pts',(7.71611241359684,-0.0370681275469361,
-0.151299690109517));
#13630=CARTESIAN_POINT('Ctrl Pts',(7.54346413841113,-0.284110713751843,
-0.166999702844742));
#13631=CARTESIAN_POINT('Ctrl Pts',(7.24217056726241,-0.276388931451618,
-0.182699715579967));
#13632=CARTESIAN_POINT('Ctrl Pts',(7.0824039775304,-0.020826327520145,-0.198399728315193));
#13633=CARTESIAN_POINT('Ctrl Pts',(7.20742887977719,0.253411337384138,-0.214099741050418));
#13634=CARTESIAN_POINT('Ctrl Pts',(7.50513410748264,0.300412677844047,-0.229799753785643));
#13635=CARTESIAN_POINT('Ctrl Pts',(7.70856459494988,0.0780310618225991,
-0.245499766520869));
#13636=CARTESIAN_POINT('Ctrl Pts',(7.63530223870985,-0.214321742927024,
-0.261199779256094));
#13637=CARTESIAN_POINT('Ctrl Pts',(7.35104211317455,-0.314490191131576,
-0.276899791991319));
#13638=CARTESIAN_POINT('Ctrl Pts',(7.11068299168808,-0.132652264669645,
-0.292599804726545));
#13639=CARTESIAN_POINT('Ctrl Pts',(7.12975720849912,0.168136218544819,-0.30829981746177));
#13640=CARTESIAN_POINT('Ctrl Pts',(7.39116072836547,0.318155342350428,-0.323999830196996));
#13641=CARTESIAN_POINT('Ctrl Pts',(7.66049050824145,0.182881518035819,-0.339699842932221));
#13642=CARTESIAN_POINT('Ctrl Pts',(7.6962359501787,-0.11638391779237,-0.355399855667446));
#13643=CARTESIAN_POINT('Ctrl Pts',(7.4663437737136,-0.311286778098894,-0.371099868402672));
#13644=CARTESIAN_POINT('Ctrl Pts',(7.17696049884618,-0.227055798078962,
-0.386799881137897));
#13645=CARTESIAN_POINT('Ctrl Pts',(7.08757888442605,0.0607782943142372,
-0.402499893873122));
#13646=CARTESIAN_POINT('Ctrl Pts',(7.27834828156687,0.294111907157829,-0.418199906608348));
#13647=CARTESIAN_POINT('Ctrl Pts',(7.57820394169864,0.263712551203101,-0.433899919343573));
#13648=CARTESIAN_POINT('Ctrl Pts',(7.71826241770918,-0.00316037923070726,
-0.449599932078799));
#13649=CARTESIAN_POINT('Ctrl Pts',(7.57293193046229,-0.267199367543656,
-0.465299944814024));
#13650=CARTESIAN_POINT('Ctrl Pts',(7.27253172219081,-0.291638119074134,
-0.480999957549249));
#13651=CARTESIAN_POINT('Ctrl Pts',(7.08643354139474,-0.0545621724118729,
-0.496699970284474));
#13652=CARTESIAN_POINT('Ctrl Pts',(7.18151341247548,0.231440199775832,-0.5123999830197));
#13653=CARTESIAN_POINT('Ctrl Pts',(7.47251230220066,0.309907920296823,-0.528099995754925));
#13654=CARTESIAN_POINT('Ctrl Pts',(7.69848871580723,0.110478244018884,-0.543800008490151));
#13655=CARTESIAN_POINT('Ctrl Pts',(7.65680743253023,-0.188018350601305,
-0.559500021225375));
#13656=CARTESIAN_POINT('Ctrl Pts',(7.38484446453224,-0.31791705208021,-0.575200033960601));
#13657=CARTESIAN_POINT('Ctrl Pts',(7.1264716030647,-0.162736552367599,-0.590900046695826));
#13658=CARTESIAN_POINT('Ctrl Pts',(7.11337429440789,0.138371514991572,-0.606600059431052));
#13659=CARTESIAN_POINT('Ctrl Pts',(7.35729697512741,0.31540023517011,-0.622300072166276));
#13660=CARTESIAN_POINT('Ctrl Pts',(7.63951192962648,0.209607107886287,-0.638000084901503));
#13661=CARTESIAN_POINT('Ctrl Pts',(7.70695411460156,-0.0841438720646569,
-0.653700097636727));
#13662=CARTESIAN_POINT('Ctrl Pts',(7.49914785125683,-0.302439918856771,
-0.669400110371954));
#13663=CARTESIAN_POINT('Ctrl Pts',(7.20243425217937,-0.249539860036695,
-0.685100123107178));
#13664=CARTESIAN_POINT('Ctrl Pts',(7.08288077581068,0.0271344069887835,
-0.700800135842404));
#13665=CARTESIAN_POINT('Ctrl Pts',(7.24768909014338,0.279457987057277,-0.716500148577629));
#13666=CARTESIAN_POINT('Ctrl Pts',(7.54908021334818,0.281227240822539,-0.732200161312854));
#13667=CARTESIAN_POINT('Ctrl Pts',(7.71678130076761,0.0307400084511485,
-0.74790017404808));
#13668=CARTESIAN_POINT('Ctrl Pts',(7.6004384294007,-0.247156051765875,-0.763600186783306));
#13669=CARTESIAN_POINT('Ctrl Pts',(7.30432695014238,-0.303740799376059,
-0.77930019951853));
#13670=CARTESIAN_POINT('Ctrl Pts',(7.09407063148472,-0.0873080033765519,
-0.795000212253756));
#13671=CARTESIAN_POINT('Ctrl Pts',(7.13681201524657,0.108091940906003,-0.805466887410573));
#13672=CARTESIAN_POINT('Ctrl Pts',(7.19456684496579,0.175642532122687,-0.810700224988981));
#13673=CARTESIAN_POINT('Ctrl Pts',(7.33498000020249,-0.243208680203507,
0.0321006749669432));
#13674=CARTESIAN_POINT('Ctrl Pts',(7.25500804955002,-0.221828784507026,
0.0268673373885347));
#13675=CARTESIAN_POINT('Ctrl Pts',(7.11910692324936,-0.0943914838419598,
0.0164006622317178));
#13676=CARTESIAN_POINT('Ctrl Pts',(7.16630818318082,0.182672232061242,0.000700649496492524));
#13677=CARTESIAN_POINT('Ctrl Pts',(7.42345550607431,0.295466755710189,-0.0149993632387329));
#13678=CARTESIAN_POINT('Ctrl Pts',(7.65937763866384,0.143538181525481,-0.0306993759739581));
#13679=CARTESIAN_POINT('Ctrl Pts',(7.66280862857218,-0.137213324645103,
-0.0463993887091836));
#13680=CARTESIAN_POINT('Ctrl Pts',(7.43052937409362,-0.294869395295694,
-0.0620994014444088));
#13681=CARTESIAN_POINT('Ctrl Pts',(7.1708975499979,-0.18814048140792,-0.0777994141796343));
#13682=CARTESIAN_POINT('Ctrl Pts',(7.11669248307145,0.0873093075356722,
-0.0934994269148595));
#13683=CARTESIAN_POINT('Ctrl Pts',(7.31653773934246,0.284461309572235,-0.109199439650085));
#13684=CARTESIAN_POINT('Ctrl Pts',(7.59122155231358,0.22653744468535,-0.12489945238531));
#13685=CARTESIAN_POINT('Ctrl Pts',(7.69443657935378,-0.0345263653324579,
-0.140599465120536));
#13686=CARTESIAN_POINT('Ctrl Pts',(7.53362679969785,-0.264629236678892,
-0.156299477855761));
#13687=CARTESIAN_POINT('Ctrl Pts',(7.25299293448225,-0.257436937138601,
-0.171999490590986));
#13688=CARTESIAN_POINT('Ctrl Pts',(7.10418154286223,-0.0193982658439779,
-0.187699503326212));
#13689=CARTESIAN_POINT('Ctrl Pts',(7.220633485172,0.236034917135561,-0.203399516061437));
#13690=CARTESIAN_POINT('Ctrl Pts',(7.49792505972285,0.27981337478167,-0.219099528796662));
#13691=CARTESIAN_POINT('Ctrl Pts',(7.68740631477572,0.0726804704218018,
-0.234799541531887));
#13692=CARTESIAN_POINT('Ctrl Pts',(7.61916755970354,-0.199625696917599,
-0.250499554267113));
#13693=CARTESIAN_POINT('Ctrl Pts',(7.35439915641003,-0.29292559271397,-0.266199567002338));
#13694=CARTESIAN_POINT('Ctrl Pts',(7.13052146447854,-0.123556296345501,
-0.281899579737564));
#13695=CARTESIAN_POINT('Ctrl Pts',(7.14828776187822,0.156607114825152,-0.297599592472789));
#13696=CARTESIAN_POINT('Ctrl Pts',(7.39176683739043,0.296339424443684,-0.313299605208015));
#13697=CARTESIAN_POINT('Ctrl Pts',(7.64262866911187,0.170341328848187,-0.32899961794324));
#13698=CARTESIAN_POINT('Ctrl Pts',(7.67592304541218,-0.108403470324582,
-0.344699630678465));
#13699=CARTESIAN_POINT('Ctrl Pts',(7.46179457988185,-0.289941837774174,
-0.360399643413691));
#13700=CARTESIAN_POINT('Ctrl Pts',(7.19225432170386,-0.211486577664347,
-0.376099656148916));
#13701=CARTESIAN_POINT('Ctrl Pts',(7.10900160629311,0.0566107255112876,
-0.391799668884141));
#13702=CARTESIAN_POINT('Ctrl Pts',(7.28668994222529,0.273944648061849,-0.407499681619367));
#13703=CARTESIAN_POINT('Ctrl Pts',(7.56598449400986,0.245629776526043,-0.423199694354592));
#13704=CARTESIAN_POINT('Ctrl Pts',(7.69643915764304,-0.00294367196644475,
-0.438899707089818));
#13705=CARTESIAN_POINT('Ctrl Pts',(7.56107398468478,-0.248877501803473,
-0.454599719825042));
#13706=CARTESIAN_POINT('Ctrl Pts',(7.28127222443683,-0.271640487674342,
-0.470299732560268));
#13707=CARTESIAN_POINT('Ctrl Pts',(7.10793479945536,-0.0508208432065944,
-0.485999745295493));
#13708=CARTESIAN_POINT('Ctrl Pts',(7.19649504195857,0.215570340853052,-0.501699758030719));
#13709=CARTESIAN_POINT('Ctrl Pts',(7.46754013225262,0.28865752827795,-0.517399770765943));
#13710=CARTESIAN_POINT('Ctrl Pts',(7.67802133885851,0.102902748714636,-0.53309978350117));
#13711=CARTESIAN_POINT('Ctrl Pts',(7.63919814197256,-0.175125928706463,
-0.548799796236394));
#13712=CARTESIAN_POINT('Ctrl Pts',(7.38588367988897,-0.29611747374185,-0.564499808971621));
#13713=CARTESIAN_POINT('Ctrl Pts',(7.14522745047125,-0.151577703860923,
-0.580199821706845));
#13714=CARTESIAN_POINT('Ctrl Pts',(7.13302822451941,0.128883377563526,-0.595899834442072));
#13715=CARTESIAN_POINT('Ctrl Pts',(7.36022512235921,0.293773235015386,-0.611599847177295));
#13716=CARTESIAN_POINT('Ctrl Pts',(7.62308859203355,0.195234344491729,-0.627299859912523));
#13717=CARTESIAN_POINT('Ctrl Pts',(7.68590626509567,-0.0783741251487107,
-0.642999872647746));
#13718=CARTESIAN_POINT('Ctrl Pts',(7.49234928120087,-0.281701607839398,
-0.658699885382973));
#13719=CARTESIAN_POINT('Ctrl Pts',(7.21598133928404,-0.232428907063839,
-0.674399898118197));
#13720=CARTESIAN_POINT('Ctrl Pts',(7.10462564707531,0.0252738001828684,
-0.690099910853423));
#13721=CARTESIAN_POINT('Ctrl Pts',(7.25813305214379,0.260295547542712,-0.705799923588648));
#13722=CARTESIAN_POINT('Ctrl Pts',(7.53885778026912,0.26194348354347,-0.721499936323873));
#13723=CARTESIAN_POINT('Ctrl Pts',(7.69505960091847,0.0286321654840352,
-0.737199949059099));
#13724=CARTESIAN_POINT('Ctrl Pts',(7.58669436246517,-0.230208556571718,
-0.752899961794324));
#13725=CARTESIAN_POINT('Ctrl Pts',(7.31088725299997,-0.282913286956612,
-0.768599974529549));
#13726=CARTESIAN_POINT('Ctrl Pts',(7.11504821413188,-0.0813212919160645,
-0.784299987264775));
#13727=CARTESIAN_POINT('Ctrl Pts',(7.15485882039215,0.10068007445182,-0.794766662421592));
#13728=CARTESIAN_POINT('Ctrl Pts',(7.2086534003335,0.163598720337497,-0.8));
#13729=CARTESIAN_POINT('Ctrl Pts',(7.14840641220525,0.000201202115797984,
-0.0887416697508019));
#13730=CARTESIAN_POINT('Ctrl Pts',(7.14821094317882,0.0253219375521799,
-0.0903275888054877));
#13731=CARTESIAN_POINT('Ctrl Pts',(7.15167836398483,0.0503900083073383,
-0.0919135078601736));
#13732=CARTESIAN_POINT('Ctrl Pts',(7.15903420360436,0.0742596763845007,
-0.0934994269148595));
#13733=CARTESIAN_POINT('Ctrl Pts',(7.18330756849512,0.15302664154786,-0.098732764493268));
#13734=CARTESIAN_POINT('Ctrl Pts',(7.24992265391879,0.218743975560048,-0.103966102071676));
#13735=CARTESIAN_POINT('Ctrl Pts',(7.32901083212581,0.241948665084994,-0.109199439650085));
#13736=CARTESIAN_POINT('Ctrl Pts',(7.40809901033283,0.26515335460994,-0.114432777228493));
#13737=CARTESIAN_POINT('Ctrl Pts',(7.49966028132321,0.245845399647645,-0.119666114806902));
#13738=CARTESIAN_POINT('Ctrl Pts',(7.5626434213251,0.19268078716353,-0.12489945238531));
#13739=CARTESIAN_POINT('Ctrl Pts',(7.62562656132698,0.139516174679414,-0.130132789963719));
#13740=CARTESIAN_POINT('Ctrl Pts',(7.66003157034038,0.0524949046734784,
-0.135366127542127));
#13741=CARTESIAN_POINT('Ctrl Pts',(7.65043244490443,-0.0293662088872284,
-0.140599465120536));
#13742=CARTESIAN_POINT('Ctrl Pts',(7.64083331946847,-0.111227322447936,
-0.145832802698944));
#13743=CARTESIAN_POINT('Ctrl Pts',(7.58723005958316,-0.187928279563414,
-0.151066140277352));
#13744=CARTESIAN_POINT('Ctrl Pts',(7.51365611877124,-0.225080041531105,
-0.156299477855761));
#13745=CARTESIAN_POINT('Ctrl Pts',(7.44008217795932,-0.262231803498795,
-0.161532815434169));
#13746=CARTESIAN_POINT('Ctrl Pts',(7.34653755622078,-0.259834370318698,
-0.166766153012578));
#13747=CARTESIAN_POINT('Ctrl Pts',(7.27496334674818,-0.218962541846212,
-0.171999490590986));
#13748=CARTESIAN_POINT('Ctrl Pts',(7.20338913727558,-0.178090713373726,
-0.177232828169395));
#13749=CARTESIAN_POINT('Ctrl Pts',(7.1537853400689,-0.0987444896088522,
-0.182466165747803));
#13750=CARTESIAN_POINT('Ctrl Pts',(7.14839209851719,-0.0164991805631585,
-0.187699503326212));
#13751=CARTESIAN_POINT('Ctrl Pts',(7.14803409528754,-0.0110397391529513,
-0.188046892134408));
#13752=CARTESIAN_POINT('Ctrl Pts',(7.14787089706648,-0.00556752350083036,
-0.188394280942605));
#13753=CARTESIAN_POINT('Ctrl Pts',(7.14789741337032,-9.36993803829212E-5,
-0.188741669750802));
#13754=CARTESIAN_POINT('Ctrl Pts',(7.32062007174671,-0.29692229537457,0.));
#13755=CARTESIAN_POINT('Ctrl Pts',(7.30380884409489,-0.290772673204267,
-8.6947763400151E-19));
#13756=CARTESIAN_POINT('Ctrl Pts',(7.28766915137083,-0.28307124049188,-5.12459696186606E-17));
#13757=CARTESIAN_POINT('Ctrl Pts',(7.27233060098557,-0.274000231430978,
-4.7271214720368E-17));
#13758=CARTESIAN_POINT('Ctrl Pts',(7.26235488632148,-0.26810073011996,-4.46861581322844E-17));
#13759=CARTESIAN_POINT('Ctrl Pts',(7.25271848455557,-0.261620831522484,
6.78577354371941E-18));
#13760=CARTESIAN_POINT('Ctrl Pts',(7.24346467188118,-0.254602044943363,
0.));
#13761=CARTESIAN_POINT('Ctrl Pts',(7.23605088975924,-0.24897887573852,-5.43648854284865E-18));
#13762=CARTESIAN_POINT('Ctrl Pts',(7.22888277290176,-0.243009665080752,
-2.33933283858092E-17));
#13763=CARTESIAN_POINT('Ctrl Pts',(7.22198623884541,-0.236713795342446,
-2.68882138776405E-17));
#13764=CARTESIAN_POINT('Ctrl Pts',(7.21845932875887,-0.233494066953934,
-2.86755097557909E-17));
#13765=CARTESIAN_POINT('Ctrl Pts',(7.21500977674086,-0.230194526695087,
3.15297170846717E-17));
#13766=CARTESIAN_POINT('Ctrl Pts',(7.21164329955151,-0.226821462504723,
3.20923843055709E-17));
#13767=CARTESIAN_POINT('Ctrl Pts',(7.19928407775938,-0.214438058102124,
3.41580834287554E-17));
#13768=CARTESIAN_POINT('Ctrl Pts',(7.18802725117541,-0.201052984273089,
5.78707788030305E-17));
#13769=CARTESIAN_POINT('Ctrl Pts',(7.17802303391905,-0.186814057526815,
8.32667268468867E-17));
#13770=CARTESIAN_POINT('Ctrl Pts',(7.17173408520147,-0.177863044388453,
9.92313756334403E-17));
#13771=CARTESIAN_POINT('Ctrl Pts',(7.16594094488153,-0.16857400717693,1.38900089258037E-17));
#13772=CARTESIAN_POINT('Ctrl Pts',(7.16069111243859,-0.15898037881098,6.93889390390723E-18));
#13773=CARTESIAN_POINT('Ctrl Pts',(7.15844635045079,-0.154878264597813,
3.96668499180442E-18));
#13774=CARTESIAN_POINT('Ctrl Pts',(7.15630103067416,-0.150720445577065,
4.11107772410956E-17));
#13775=CARTESIAN_POINT('Ctrl Pts',(7.15425938021799,-0.146509500605675,
4.16333634234434E-17));
#13776=CARTESIAN_POINT('Ctrl Pts',(7.15231306464394,-0.14249518573874,4.21315474404055E-17));
#13777=CARTESIAN_POINT('Ctrl Pts',(7.15046487911057,-0.138440587136871,
2.62921600658027E-17));
#13778=CARTESIAN_POINT('Ctrl Pts',(7.14871822055084,-0.134350184983525,
2.77555756156289E-17));
#13779=CARTESIAN_POINT('Ctrl Pts',(7.14246237732693,-0.119699975043201,
3.29969539034211E-17));
#13780=CARTESIAN_POINT('Ctrl Pts',(7.13750157461332,-0.1045828565666,7.60800602575303E-18));
#13781=CARTESIAN_POINT('Ctrl Pts',(7.13397523077828,-0.0891087999794577,
6.93889390390723E-18));
#13782=CARTESIAN_POINT('Ctrl Pts',(7.13145831420858,-0.0780642418629789,
6.30212507089961E-18));
#13783=CARTESIAN_POINT('Ctrl Pts',(7.12967323652615,-0.0668374439349906,
-2.87387945550391E-17));
#13784=CARTESIAN_POINT('Ctrl Pts',(7.12860812217214,-0.0554971960327241,
-4.16333634234434E-17));
#13785=CARTESIAN_POINT('Ctrl Pts',(7.12819480164633,-0.051096581950223,
-4.66371359898912E-17));
#13786=CARTESIAN_POINT('Ctrl Pts',(7.12789000373709,-0.046678913727008,
-5.89876804906217E-18));
#13787=CARTESIAN_POINT('Ctrl Pts',(7.1276934258001,-0.0422483700808671,
-1.04083408558608E-17));
#13788=CARTESIAN_POINT('Ctrl Pts',(7.12749092575898,-0.0376843519398602,
-1.50537689888955E-17));
#13789=CARTESIAN_POINT('Ctrl Pts',(7.12740372610782,-0.0331164650875104,
1.05127888270269E-18));
#13790=CARTESIAN_POINT('Ctrl Pts',(7.12743015237759,-0.0285512580926939,
3.46944695195361E-18));
#13791=CARTESIAN_POINT('Ctrl Pts',(7.12752823277688,-0.0116076134235948,
1.24444135990454E-17));
#13792=CARTESIAN_POINT('Ctrl Pts',(7.12918689135693,0.00531003058111619,
3.46252004887064E-17));
#13793=CARTESIAN_POINT('Ctrl Pts',(7.13235152789467,0.0219706470489435,
6.59194920871187E-17));
#13794=CARTESIAN_POINT('Ctrl Pts',(7.13400565404307,0.0306789966553936,
8.22767278743674E-17));
#13795=CARTESIAN_POINT('Ctrl Pts',(7.13607212944229,0.0393168936655102,
2.69042433030263E-17));
#13796=CARTESIAN_POINT('Ctrl Pts',(7.13854854623344,0.0478483384877713,
3.12250225675825E-17));
#13797=CARTESIAN_POINT('Ctrl Pts',(7.13999886673045,0.0528448032747235,
3.37554991629673E-17));
#13798=CARTESIAN_POINT('Ctrl Pts',(7.14159044784196,0.0578063658571401,
-8.00558532562018E-17));
#13799=CARTESIAN_POINT('Ctrl Pts',(7.1433214609991,0.0627200384290504,-5.89805981832114E-17));
#13800=CARTESIAN_POINT('Ctrl Pts',(7.1486420056914,0.0778229938366053,5.79755561356752E-18));
#13801=CARTESIAN_POINT('Ctrl Pts',(7.15525121899922,0.0924060906234471,
2.3609484991885E-18));
#13802=CARTESIAN_POINT('Ctrl Pts',(7.16312552449122,0.106254752470274,3.46944695195361E-17));
#13803=CARTESIAN_POINT('Ctrl Pts',(7.16719213282866,0.113406758927964,5.139280136525E-17));
#13804=CARTESIAN_POINT('Ctrl Pts',(7.171600828714,0.120367188403168,6.62813824659908E-17));
#13805=CARTESIAN_POINT('Ctrl Pts',(7.17633091943804,0.127074857793874,3.81639164714898E-17));
#13806=CARTESIAN_POINT('Ctrl Pts',(7.18357704399351,0.137350476321644,-4.90981565480567E-18));
#13807=CARTESIAN_POINT('Ctrl Pts',(7.19158181099666,0.14704579400106,-4.84899983333435E-17));
#13808=CARTESIAN_POINT('Ctrl Pts',(7.20034135671288,0.156042628024828,-4.16333634234434E-17));
#13809=CARTESIAN_POINT('Ctrl Pts',(7.20292789437632,0.15869923269453,-3.96087213913729E-17));
#13810=CARTESIAN_POINT('Ctrl Pts',(7.20558033511274,0.16129479584369,-2.29970654385668E-17));
#13811=CARTESIAN_POINT('Ctrl Pts',(7.20829596415884,0.163828130483802,-2.08166817117217E-17));
#13812=CARTESIAN_POINT('Origin',(0.,7.4,0.220842344717745));
#13813=CARTESIAN_POINT('Ctrl Pts',(-0.307720586104713,7.40015430359934,
-0.0291576552822542));
#13814=CARTESIAN_POINT('Ctrl Pts',(-0.307784268539838,7.41004356083263,
-0.0296715621794888));
#13815=CARTESIAN_POINT('Ctrl Pts',(-0.302900304337239,7.52057842373192,
-0.0354188066551319));
#13816=CARTESIAN_POINT('Ctrl Pts',(-0.169525066073537,7.71979475374946,
-0.0463993887091835));
#13817=CARTESIAN_POINT('Ctrl Pts',(0.173198823302611,7.71778284450742,-0.0620994014444088));
#13818=CARTESIAN_POINT('Ctrl Pts',(0.360608951848397,7.43085562333351,-0.0777994141796342));
#13819=CARTESIAN_POINT('Ctrl Pts',(0.224659911311872,7.11623824447284,-0.0934994269148595));
#13820=CARTESIAN_POINT('Ctrl Pts',(-0.112744986006889,7.05608347580814,
-0.109199439650085));
#13821=CARTESIAN_POINT('Ctrl Pts',(-0.291645285757027,7.24401442263803,
-0.12108551577255));
#13822=CARTESIAN_POINT('Ctrl Pts',(-0.307476655132152,7.37231065231555,
-0.127738254316606));
#13823=CARTESIAN_POINT('Ctrl Pts',(-0.307245619935592,7.39973933390828,
-0.129157655282254));
#13824=CARTESIAN_POINT('Ctrl Pts',(-0.30701976654778,7.39969382919393,-0.0208423447177451));
#13825=CARTESIAN_POINT('Ctrl Pts',(-0.306554866839469,7.46778804886732,
-0.0243615716353136));
#13826=CARTESIAN_POINT('Ctrl Pts',(-0.251028091428161,7.63805053601396,
-0.0331141361312906));
#13827=CARTESIAN_POINT('Ctrl Pts',(0.0286357548570192,7.76072194419717,
-0.047100038205676));
#13828=CARTESIAN_POINT('Ctrl Pts',(0.316662279094702,7.57523911945597,-0.0628000509409012));
#13829=CARTESIAN_POINT('Ctrl Pts',(0.320851004579023,7.23248257807725,-0.0785000636761267));
#13830=CARTESIAN_POINT('Ctrl Pts',(0.037271918951097,7.04000744673753,-0.094200076411352));
#13831=CARTESIAN_POINT('Ctrl Pts',(-0.247682056237118,7.15714576429466,
-0.108314170091891));
#13832=CARTESIAN_POINT('Ctrl Pts',(-0.306610241848052,7.32971128185523,
-0.117194926194023));
#13833=CARTESIAN_POINT('Ctrl Pts',(-0.307159081926734,7.40024563889874,
-0.120842344717745));
#13834=CARTESIAN_POINT('Ctrl Pts',(0.191346599666507,7.56359872033749,5.55111512312578E-17));
#13835=CARTESIAN_POINT('Ctrl Pts',(0.245141179607854,7.50068007445182,-0.00523333757840839));
#13836=CARTESIAN_POINT('Ctrl Pts',(0.284951890218192,7.31867881897261,-0.0157000127352253));
#13837=CARTESIAN_POINT('Ctrl Pts',(0.0891126990759621,7.11708667871666,
-0.0314000254704506));
#13838=CARTESIAN_POINT('Ctrl Pts',(-0.186694333111318,7.1697914830401,-0.047100038205676));
#13839=CARTESIAN_POINT('Ctrl Pts',(-0.295059597649767,7.42863214647761,
-0.0628000509409013));
#13840=CARTESIAN_POINT('Ctrl Pts',(-0.138857769266351,7.66194348220735,
-0.0785000636761267));
#13841=CARTESIAN_POINT('Ctrl Pts',(0.141866939210777,7.66029552986739,-0.094200076411352));
#13842=CARTESIAN_POINT('Ctrl Pts',(0.295374340744539,7.42527380242139,-0.109900089146577));
#13843=CARTESIAN_POINT('Ctrl Pts',(0.184018651936761,7.16757110150004,-0.125600101881803));
#13844=CARTESIAN_POINT('Ctrl Pts',(-0.0923492768089616,7.11829840583927,
-0.141300114617028));
#13845=CARTESIAN_POINT('Ctrl Pts',(-0.28590625237283,7.32162587781138,-0.157000127352254));
#13846=CARTESIAN_POINT('Ctrl Pts',(-0.223088581960643,7.59523433602638,
-0.172700140087479));
#13847=CARTESIAN_POINT('Ctrl Pts',(0.0397748758287548,7.69377322166141,
-0.188400152822704));
#13848=CARTESIAN_POINT('Ctrl Pts',(0.266971763504157,7.52888337186213,-0.204100165557929));
#13849=CARTESIAN_POINT('Ctrl Pts',(0.254772538082208,7.24842230290007,-0.219800178293155));
#13850=CARTESIAN_POINT('Ctrl Pts',(0.0141163194798009,7.10388253957977,
-0.23550019102838));
#13851=CARTESIAN_POINT('Ctrl Pts',(-0.239198131232389,7.22487407914503,
-0.251200203763606));
#13852=CARTESIAN_POINT('Ctrl Pts',(-0.278021326373094,7.50290274410036,
-0.266900216498831));
#13853=CARTESIAN_POINT('Ctrl Pts',(-0.0675401292199379,7.68865751531201,
-0.282600229234056));
#13854=CARTESIAN_POINT('Ctrl Pts',(0.20350494890297,7.61557033117447,-0.298300241969282));
#13855=CARTESIAN_POINT('Ctrl Pts',(0.292065187429107,7.34917915907462,-0.314000254704507));
#13856=CARTESIAN_POINT('Ctrl Pts',(0.118727770231601,7.12835952452443,-0.329700267439732));
#13857=CARTESIAN_POINT('Ctrl Pts',(-0.161073977451607,7.15112250937237,
-0.345400280174958));
#13858=CARTESIAN_POINT('Ctrl Pts',(-0.296439144331143,7.39705632816588,
-0.361100292910182));
#13859=CARTESIAN_POINT('Ctrl Pts',(-0.165984486556164,7.64562976549573,
-0.376800305645409));
#13860=CARTESIAN_POINT('Ctrl Pts',(0.113310052686424,7.67394463576013,-0.392500318380633));
#13861=CARTESIAN_POINT('Ctrl Pts',(0.29099838063931,7.4566107229691,-0.408200331115859));
#13862=CARTESIAN_POINT('Ctrl Pts',(0.207745668967121,7.18851343183269,-0.423900343851084));
#13863=CARTESIAN_POINT('Ctrl Pts',(-0.0617945771069258,7.11005817524592,
-0.43960035658631));
#13864=CARTESIAN_POINT('Ctrl Pts',(-0.275923033021548,7.29159653454344,
-0.455300369321535));
#13865=CARTESIAN_POINT('Ctrl Pts',(-0.242628658216455,7.57034132119874,
-0.471000382056761));
#13866=CARTESIAN_POINT('Ctrl Pts',(0.00823316223999692,7.69633941113648,
-0.486700394791986));
#13867=CARTESIAN_POINT('Ctrl Pts',(0.251712226818136,7.55660710779213,-0.502400407527211));
#13868=CARTESIAN_POINT('Ctrl Pts',(0.269478523420751,7.27644370920372,-0.518100420262436));
#13869=CARTESIAN_POINT('Ctrl Pts',(0.045600841541278,7.10707442043858,-0.533800432997662));
#13870=CARTESIAN_POINT('Ctrl Pts',(-0.219167549859846,7.20037431204982,
-0.549500445732887));
#13871=CARTESIAN_POINT('Ctrl Pts',(-0.287406301872761,7.4726804671522,-0.565200458468112));
#13872=CARTESIAN_POINT('Ctrl Pts',(-0.097925055319246,7.67981336222756,
-0.580900471203338));
#13873=CARTESIAN_POINT('Ctrl Pts',(0.179366506761887,7.63603490651475,-0.596600483938563));
#13874=CARTESIAN_POINT('Ctrl Pts',(0.295818443874949,7.38060173506806,-0.612300496673788));
#13875=CARTESIAN_POINT('Ctrl Pts',(0.147007058877446,7.14256307434387,-0.628000509409014));
#13876=CARTESIAN_POINT('Ctrl Pts',(-0.133626793626916,7.13537077535256,
-0.643700522144239));
#13877=CARTESIAN_POINT('Ctrl Pts',(-0.294436566257555,7.36547363593814,
-0.659400534879464));
#13878=CARTESIAN_POINT('Ctrl Pts',(-0.191221543505373,7.6265374350392,-0.67510054761469));
#13879=CARTESIAN_POINT('Ctrl Pts',(0.0834622565287631,7.68446129581186,
-0.690800560349915));
#13880=CARTESIAN_POINT('Ctrl Pts',(0.283307504842672,7.48730930545105,-0.706500573085141));
#13881=CARTESIAN_POINT('Ctrl Pts',(0.229102438696414,7.21185952364665,-0.722200585820366));
#13882=CARTESIAN_POINT('Ctrl Pts',(-0.0305293712063166,7.10513062416771,
-0.737900598555592));
#13883=CARTESIAN_POINT('Ctrl Pts',(-0.262808618747949,7.26278667022359,
-0.753600611290816));
#13884=CARTESIAN_POINT('Ctrl Pts',(-0.259377625204068,7.54353819533719,
-0.769300624026042));
#13885=CARTESIAN_POINT('Ctrl Pts',(-0.0234555043215238,7.69546670643878,
-0.785000636761267));
#13886=CARTESIAN_POINT('Ctrl Pts',(0.233691796768955,7.58267228749613,-0.800700649496493));
#13887=CARTESIAN_POINT('Ctrl Pts',(0.28089309993379,7.30560836566625,-0.816400662231718));
#13888=CARTESIAN_POINT('Ctrl Pts',(0.144991950449973,7.17817121549297,-0.826867337388535));
#13889=CARTESIAN_POINT('Ctrl Pts',(0.0650199997975051,7.15679131979649,
-0.832100674966943));
#13890=CARTESIAN_POINT('Ctrl Pts',(0.20543315503421,7.57564253212268,0.0107002249889811));
#13891=CARTESIAN_POINT('Ctrl Pts',(0.26318798475343,7.508091940906,0.00546688741057267));
#13892=CARTESIAN_POINT('Ctrl Pts',(0.305929480547396,7.31269211567552,-0.00499978774624422));
#13893=CARTESIAN_POINT('Ctrl Pts',(0.0956729984054867,7.09625916377015,
-0.0206998004814696));
#13894=CARTESIAN_POINT('Ctrl Pts',(-0.200438397885882,7.15284399076208,
-0.0363998132166949));
#13895=CARTESIAN_POINT('Ctrl Pts',(-0.316781297258277,7.43073998804551,
-0.0520998259519203));
#13896=CARTESIAN_POINT('Ctrl Pts',(-0.149080201535413,7.68122723938805,
-0.0677998386871456));
#13897=CARTESIAN_POINT('Ctrl Pts',(0.152310900574722,7.67945796808074,-0.083499851422371));
#13898=CARTESIAN_POINT('Ctrl Pts',(0.317119211112491,7.42713440939209,-0.0991998641575964));
#13899=CARTESIAN_POINT('Ctrl Pts',(0.197565738395132,7.15046014915765,-0.114899876892822));
#13900=CARTESIAN_POINT('Ctrl Pts',(-0.0991478465416041,7.09756009582889,
-0.130599889628047));
#13901=CARTESIAN_POINT('Ctrl Pts',(-0.306954100942084,7.31585613111335,
-0.146299902363272));
#13902=CARTESIAN_POINT('Ctrl Pts',(-0.239511918812032,7.60960709879773,
-0.161999915098498));
#13903=CARTESIAN_POINT('Ctrl Pts',(0.0427030229271706,7.71540022083304,
-0.177699927833723));
#13904=CARTESIAN_POINT('Ctrl Pts',(0.28662569273399,7.53837150887044,-0.193399940568948));
#13905=CARTESIAN_POINT('Ctrl Pts',(0.273528384646088,7.23726345489113,-0.209099953304174));
#13906=CARTESIAN_POINT('Ctrl Pts',(0.0151555347900653,7.08208296222211,
-0.224799966039399));
#13907=CARTESIAN_POINT('Ctrl Pts',(-0.256807420999381,7.21198165782819,
-0.240499978774624));
#13908=CARTESIAN_POINT('Ctrl Pts',(-0.298488702402679,7.51047823906491,
-0.25619999150985));
#13909=CARTESIAN_POINT('Ctrl Pts',(-0.0725122989447028,7.70990790637636,
-0.271900004245075));
#13910=CARTESIAN_POINT('Ctrl Pts',(0.218486577713304,7.63144018938473,-0.287600016980301));
#13911=CARTESIAN_POINT('Ctrl Pts',(0.313566444524186,7.34543783003727,-0.303300029715526));
#13912=CARTESIAN_POINT('Ctrl Pts',(0.127468272085129,7.10836189402269,-0.319000042450751));
#13913=CARTESIAN_POINT('Ctrl Pts',(-0.172931922696637,7.13280064445492,
-0.334700055185977));
#13914=CARTESIAN_POINT('Ctrl Pts',(-0.318262403417289,7.39683962091136,
-0.350400067921201));
#13915=CARTESIAN_POINT('Ctrl Pts',(-0.178203933696214,7.66371253936076,
-0.366100080656428));
#13916=CARTESIAN_POINT('Ctrl Pts',(0.121651712970258,7.69411189395048,-0.381800093391652));
#13917=CARTESIAN_POINT('Ctrl Pts',(0.312421101544368,7.4607782915849,-0.397500106126878));
#13918=CARTESIAN_POINT('Ctrl Pts',(0.223039491138021,7.17294421211722,-0.413200118862104));
#13919=CARTESIAN_POINT('Ctrl Pts',(-0.0663437707343935,7.08871323587971,
-0.428900131597328));
#13920=CARTESIAN_POINT('Ctrl Pts',(-0.296235936875898,7.28361608743404,
-0.444600144332554));
#13921=CARTESIAN_POINT('Ctrl Pts',(-0.260490496543942,7.58288150982323,
-0.460300157067779));
#13922=CARTESIAN_POINT('Ctrl Pts',(0.0088392712377377,7.71815532806358,
-0.476000169803004));
#13923=CARTESIAN_POINT('Ctrl Pts',(0.270242779365091,7.56813621099405,-0.49170018253823));
#13924=CARTESIAN_POINT('Ctrl Pts',(0.289316995320379,7.2673477412881,-0.507400195273455));
#13925=CARTESIAN_POINT('Ctrl Pts',(0.0489578846259453,7.08550982298924,
-0.523100208008681));
#13926=CARTESIAN_POINT('Ctrl Pts',(-0.235302228141484,7.18567826670055,
-0.538800220743906));
#13927=CARTESIAN_POINT('Ctrl Pts',(-0.308564581097026,7.4780310583123,-0.554500233479132));
#13928=CARTESIAN_POINT('Ctrl Pts',(-0.105134102754863,7.70041266436573,
-0.570200246214357));
#13929=CARTESIAN_POINT('Ctrl Pts',(0.192571111562895,7.65341132598145,-0.585900258949582));
#13930=CARTESIAN_POINT('Ctrl Pts',(0.31759600823039,7.37917367345902,-0.601600271684807));
#13931=CARTESIAN_POINT('Ctrl Pts',(0.157829425608444,7.12361108087618,-0.617300284420032));
#13932=CARTESIAN_POINT('Ctrl Pts',(-0.14346413189326,7.11588929916533,-0.633000297155258));
#13933=CARTESIAN_POINT('Ctrl Pts',(-0.316112399536496,7.36293187381722,
-0.648700309890483));
#13934=CARTESIAN_POINT('Ctrl Pts',(-0.205298892487695,7.64321466958163,
-0.664400322625709));
#13935=CARTESIAN_POINT('Ctrl Pts',(0.0896065815376993,7.70540276955849,
-0.680100335360935));
#13936=CARTESIAN_POINT('Ctrl Pts',(0.304164038797326,7.49373684253556,-0.695800348096159));
#13937=CARTESIAN_POINT('Ctrl Pts',(0.245968503696772,7.19800899668837,-0.711500360831385));
#13938=CARTESIAN_POINT('Ctrl Pts',(-0.0327768826781086,7.08342292831035,
-0.72720037356661));
#13939=CARTESIAN_POINT('Ctrl Pts',(-0.282156065556801,7.25268529831287,
-0.742900386301836));
#13940=CARTESIAN_POINT('Ctrl Pts',(-0.278472489105221,7.55410519124682,
-0.75860039903706));
#13941=CARTESIAN_POINT('Ctrl Pts',(-0.025182251809477,7.71721837658509,
-0.774300411772287));
#13942=CARTESIAN_POINT('Ctrl Pts',(0.250895721165319,7.5961202572873,-0.790000424507511));
#13943=CARTESIAN_POINT('Ctrl Pts',(0.30157189021028,7.29865944164248,-0.805700437242738));
#13944=CARTESIAN_POINT('Ctrl Pts',(0.155665968914083,7.1618406224197,-0.816167112399554));
#13945=CARTESIAN_POINT('Ctrl Pts',(0.0698066426160968,7.13888678140614,
-0.821400449977962));
#13946=CARTESIAN_POINT('Ctrl Pts',(0.219519710401913,7.58768634390787,0.0214004499779622));
#13947=CARTESIAN_POINT('Ctrl Pts',(0.281234789899007,7.51550380736018,0.0161671123995537));
#13948=CARTESIAN_POINT('Ctrl Pts',(0.3269070708766,7.30670541237844,0.00570043724273685));
#13949=CARTESIAN_POINT('Ctrl Pts',(0.102233297735012,7.07543164882364,-0.00999957549248853));
#13950=CARTESIAN_POINT('Ctrl Pts',(-0.214182462660446,7.13589649848406,
-0.0256995882277138));
#13951=CARTESIAN_POINT('Ctrl Pts',(-0.338502996866787,7.43284782961341,
-0.0413996009629392));
#13952=CARTESIAN_POINT('Ctrl Pts',(-0.159302633804475,7.70051099656875,
-0.0570996136981645));
#13953=CARTESIAN_POINT('Ctrl Pts',(0.162754861938666,7.69862040629408,-0.0727996264333899));
#13954=CARTESIAN_POINT('Ctrl Pts',(0.338864081480445,7.4289950163628,-0.0884996391686152));
#13955=CARTESIAN_POINT('Ctrl Pts',(0.211112824853502,7.13334919681524,-0.104199651903841));
#13956=CARTESIAN_POINT('Ctrl Pts',(-0.105946416274246,7.07682178581851,
-0.119899664639066));
#13957=CARTESIAN_POINT('Ctrl Pts',(-0.328001949511339,7.31008638441533,
-0.135599677374291));
#13958=CARTESIAN_POINT('Ctrl Pts',(-0.255935255663421,7.62397986156908,
-0.151299690109517));
#13959=CARTESIAN_POINT('Ctrl Pts',(0.0456311700255866,7.73702722000468,
-0.166999702844742));
#13960=CARTESIAN_POINT('Ctrl Pts',(0.306279621963823,7.54785964587876,-0.182699715579967));
#13961=CARTESIAN_POINT('Ctrl Pts',(0.292284231209968,7.22610460688219,-0.198399728315193));
#13962=CARTESIAN_POINT('Ctrl Pts',(0.0161947501003294,7.06028338486446,
-0.214099741050418));
#13963=CARTESIAN_POINT('Ctrl Pts',(-0.274416710766373,7.19908923651137,
-0.229799753785644));
#13964=CARTESIAN_POINT('Ctrl Pts',(-0.318956078432264,7.51805373402946,
-0.245499766520868));
#13965=CARTESIAN_POINT('Ctrl Pts',(-0.0774844686694676,7.73115829744071,
-0.261199779256094));
#13966=CARTESIAN_POINT('Ctrl Pts',(0.233468206523639,7.64731004759499,-0.276899791991319));
#13967=CARTESIAN_POINT('Ctrl Pts',(0.335067701619265,7.34169650099994,-0.292599804726545));
#13968=CARTESIAN_POINT('Ctrl Pts',(0.136208773938657,7.08836426352094,-0.30829981746177));
#13969=CARTESIAN_POINT('Ctrl Pts',(-0.184789867941668,7.11447877953749,
-0.323999830196996));
#13970=CARTESIAN_POINT('Ctrl Pts',(-0.340085662503434,7.39662291365683,
-0.33969984293222));
#13971=CARTESIAN_POINT('Ctrl Pts',(-0.190423380836264,7.68179531322579,
-0.355399855667447));
#13972=CARTESIAN_POINT('Ctrl Pts',(0.129993373254091,7.71427915214083,-0.371099868402671));
#13973=CARTESIAN_POINT('Ctrl Pts',(0.333843822449427,7.4649458602007,-0.386799881137897));
#13974=CARTESIAN_POINT('Ctrl Pts',(0.23833331330892,7.15737499240176,-0.402499893873122));
#13975=CARTESIAN_POINT('Ctrl Pts',(-0.0708929643618612,7.06736829651351,
-0.418199906608347));
#13976=CARTESIAN_POINT('Ctrl Pts',(-0.316548840730248,7.27563564032462,
-0.433899919343573));
#13977=CARTESIAN_POINT('Ctrl Pts',(-0.27835233487143,7.59542169844773,-0.449599932078798));
#13978=CARTESIAN_POINT('Ctrl Pts',(0.00944538023547856,7.73997124499067,
-0.465299944814023));
#13979=CARTESIAN_POINT('Ctrl Pts',(0.288773331912047,7.57966531419596,-0.48099995754925));
#13980=CARTESIAN_POINT('Ctrl Pts',(0.309155467220007,7.25825177337248,-0.496699970284473));
#13981=CARTESIAN_POINT('Ctrl Pts',(0.0523149277106133,7.0639452255399,-0.512399983019701));
#13982=CARTESIAN_POINT('Ctrl Pts',(-0.251436906423123,7.17098222135129,
-0.528099995754924));
#13983=CARTESIAN_POINT('Ctrl Pts',(-0.329722860321289,7.48338164947239,
-0.543800008490151));
#13984=CARTESIAN_POINT('Ctrl Pts',(-0.112343150190481,7.72101196650389,
-0.559500021225375));
#13985=CARTESIAN_POINT('Ctrl Pts',(0.205775716363902,7.67078774544814,-0.575200033960602));
#13986=CARTESIAN_POINT('Ctrl Pts',(0.339373572585832,7.37774561185,-0.590900046695826));
#13987=CARTESIAN_POINT('Ctrl Pts',(0.168651792339442,7.10465908740848,-0.606600059431052));
#13988=CARTESIAN_POINT('Ctrl Pts',(-0.153301470159604,7.09640782297811,
-0.622300072166277));
#13989=CARTESIAN_POINT('Ctrl Pts',(-0.337788232815437,7.36039011169628,
-0.638000084901502));
#13990=CARTESIAN_POINT('Ctrl Pts',(-0.219376241470017,7.65989190412407,
-0.653700097636728));
#13991=CARTESIAN_POINT('Ctrl Pts',(0.0957509065466354,7.72634424330511,
-0.669400110371953));
#13992=CARTESIAN_POINT('Ctrl Pts',(0.325020572751981,7.50016437962007,-0.685100123107179));
#13993=CARTESIAN_POINT('Ctrl Pts',(0.26283456869713,7.18415846973008,-0.700800135842403));
#13994=CARTESIAN_POINT('Ctrl Pts',(-0.0350243941499009,7.06171523245298,
-0.71650014857763));
#13995=CARTESIAN_POINT('Ctrl Pts',(-0.301503512365654,7.24258392640215,
-0.732200161312854));
#13996=CARTESIAN_POINT('Ctrl Pts',(-0.297567353006375,7.56467218715645,
-0.74790017404808));
#13997=CARTESIAN_POINT('Ctrl Pts',(-0.0269089992974306,7.73897004673138,
-0.763600186783305));
#13998=CARTESIAN_POINT('Ctrl Pts',(0.268099645561683,7.60956822707849,-0.779300199518531));
#13999=CARTESIAN_POINT('Ctrl Pts',(0.32225068048677,7.2917105176187,-0.795000212253756));
#14000=CARTESIAN_POINT('Ctrl Pts',(0.166339987378192,7.14551002934642,-0.805466887410573));
#14001=CARTESIAN_POINT('Ctrl Pts',(0.0745932854346885,7.12098224301578,
-0.810700224988981));
#14002=CARTESIAN_POINT('Ctrl Pts',(0.233606265769617,7.59973015569306,0.0321006749669432));
#14003=CARTESIAN_POINT('Ctrl Pts',(0.299281595044583,7.52291567381436,0.0268673373885348));
#14004=CARTESIAN_POINT('Ctrl Pts',(0.347884661205805,7.30071870908135,0.0164006622317179));
#14005=CARTESIAN_POINT('Ctrl Pts',(0.108793597064536,7.05460413387712,0.000700649496492544));
#14006=CARTESIAN_POINT('Ctrl Pts',(-0.227926527435009,7.11894900620605,
-0.0149993632387328));
#14007=CARTESIAN_POINT('Ctrl Pts',(-0.360224696475297,7.43495567118131,
-0.0306993759739581));
#14008=CARTESIAN_POINT('Ctrl Pts',(-0.169525066073537,7.71979475374946,
-0.0463993887091835));
#14009=CARTESIAN_POINT('Ctrl Pts',(0.173198823302611,7.71778284450742,-0.0620994014444088));
#14010=CARTESIAN_POINT('Ctrl Pts',(0.360608951848397,7.43085562333351,-0.0777994141796342));
#14011=CARTESIAN_POINT('Ctrl Pts',(0.224659911311872,7.11623824447284,-0.0934994269148595));
#14012=CARTESIAN_POINT('Ctrl Pts',(-0.112744986006889,7.05608347580814,
-0.109199439650085));
#14013=CARTESIAN_POINT('Ctrl Pts',(-0.349049798080593,7.30431663771729,
-0.12489945238531));
#14014=CARTESIAN_POINT('Ctrl Pts',(-0.272358592514811,7.63835262434044,
-0.140599465120536));
#14015=CARTESIAN_POINT('Ctrl Pts',(0.0485593171240025,7.7586542191763,-0.156299477855761));
#14016=CARTESIAN_POINT('Ctrl Pts',(0.325933551193656,7.55734778288709,-0.171999490590986));
#14017=CARTESIAN_POINT('Ctrl Pts',(0.311040077773849,7.21494575887322,-0.187699503326212));
#14018=CARTESIAN_POINT('Ctrl Pts',(0.0172339654105937,7.03848380750682,
-0.203399516061437));
#14019=CARTESIAN_POINT('Ctrl Pts',(-0.292026000533365,7.18619681519453,
-0.219099528796662));
#14020=CARTESIAN_POINT('Ctrl Pts',(-0.339423454461849,7.52562922899402,
-0.234799541531887));
#14021=CARTESIAN_POINT('Ctrl Pts',(-0.0824566383942325,7.75240868850505,
-0.250499554267113));
#14022=CARTESIAN_POINT('Ctrl Pts',(0.248449835333973,7.66317990580525,-0.266199567002338));
#14023=CARTESIAN_POINT('Ctrl Pts',(0.356568958714344,7.3379551719626,-0.281899579737564));
#14024=CARTESIAN_POINT('Ctrl Pts',(0.144949275792185,7.0683666330192,-0.297599592472788));
#14025=CARTESIAN_POINT('Ctrl Pts',(-0.196647813186698,7.09615691462004,
-0.313299605208015));
#14026=CARTESIAN_POINT('Ctrl Pts',(-0.36190892158958,7.39640620640232,-0.328999617943239));
#14027=CARTESIAN_POINT('Ctrl Pts',(-0.202642827976314,7.69987808709081,
-0.344699630678466));
#14028=CARTESIAN_POINT('Ctrl Pts',(0.138335033537924,7.73444641033119,-0.36039964341369));
#14029=CARTESIAN_POINT('Ctrl Pts',(0.355266543354486,7.46911342881649,-0.376099656148916));
#14030=CARTESIAN_POINT('Ctrl Pts',(0.25362713547982,7.1418057726863,-0.391799668884141));
#14031=CARTESIAN_POINT('Ctrl Pts',(-0.0754421579893288,7.0460233571473,
-0.407499681619367));
#14032=CARTESIAN_POINT('Ctrl Pts',(-0.336861744584598,7.26765519321521,
-0.423199694354592));
#14033=CARTESIAN_POINT('Ctrl Pts',(-0.296214173198918,7.60796188707222,
-0.438899707089817));
#14034=CARTESIAN_POINT('Ctrl Pts',(0.0100514892332193,7.76178716191776,
-0.454599719825043));
#14035=CARTESIAN_POINT('Ctrl Pts',(0.307303884459003,7.59119441739787,-0.470299732560268));
#14036=CARTESIAN_POINT('Ctrl Pts',(0.328993939119635,7.24915580545685,-0.485999745295493));
#14037=CARTESIAN_POINT('Ctrl Pts',(0.0556719707952805,7.04238062809055,
-0.501699758030718));
#14038=CARTESIAN_POINT('Ctrl Pts',(-0.267571584704761,7.15628617600203,
-0.517399770765944));
#14039=CARTESIAN_POINT('Ctrl Pts',(-0.350881139545554,7.48873224063248,
-0.533099783501169));
#14040=CARTESIAN_POINT('Ctrl Pts',(-0.119552197626099,7.74161126864207,
-0.548799796236395));
#14041=CARTESIAN_POINT('Ctrl Pts',(0.21898032116491,7.68816416491483,-0.56449980897162));
#14042=CARTESIAN_POINT('Ctrl Pts',(0.361151136941273,7.37631755024098,-0.580199821706846));
#14043=CARTESIAN_POINT('Ctrl Pts',(0.17947415907044,7.08570709394078,-0.59589983444207));
#14044=CARTESIAN_POINT('Ctrl Pts',(-0.163138808425949,7.0769263467909,-0.611599847177296));
#14045=CARTESIAN_POINT('Ctrl Pts',(-0.359464066094377,7.35784834957533,
-0.627299859912521));
#14046=CARTESIAN_POINT('Ctrl Pts',(-0.23345359045234,7.67656913866652,-0.642999872647747));
#14047=CARTESIAN_POINT('Ctrl Pts',(0.101895231555572,7.74728571705174,-0.658699885382972));
#14048=CARTESIAN_POINT('Ctrl Pts',(0.345877106706635,7.50659191670458,-0.674399898118198));
#14049=CARTESIAN_POINT('Ctrl Pts',(0.279700633697489,7.17030794277179,-0.690099910853422));
#14050=CARTESIAN_POINT('Ctrl Pts',(-0.0372719056216933,7.04000753659561,
-0.705799923588649));
#14051=CARTESIAN_POINT('Ctrl Pts',(-0.320850959174506,7.23248255449144,
-0.721499936323873));
#14052=CARTESIAN_POINT('Ctrl Pts',(-0.316662216907529,7.57523918306608,
-0.737199949059099));
#14053=CARTESIAN_POINT('Ctrl Pts',(-0.0286357467853838,7.76072171687769,
-0.752899961794324));
#14054=CARTESIAN_POINT('Ctrl Pts',(0.285303569958047,7.62301619686966,-0.76859997452955));
#14055=CARTESIAN_POINT('Ctrl Pts',(0.342929470763259,7.28476159359493,-0.784299987264775));
#14056=CARTESIAN_POINT('Ctrl Pts',(0.177014005842301,7.12917943627315,-0.794766662421592));
#14057=CARTESIAN_POINT('Ctrl Pts',(0.0793799282532802,7.10307770462543,
-0.8));
#14058=CARTESIAN_POINT('Ctrl Pts',(0.191346599666507,7.56359872033749,5.55111512312578E-17));
#14059=CARTESIAN_POINT('Ctrl Pts',(0.202509826020292,7.55310802872158,6.16763785454856E-17));
#14060=CARTESIAN_POINT('Ctrl Pts',(0.212570047977324,7.54158673074805,8.87136279239473E-17));
#14061=CARTESIAN_POINT('Ctrl Pts',(0.221522330388386,7.52925232800775,7.37257477290143E-17));
#14062=CARTESIAN_POINT('Ctrl Pts',(0.229528850137145,7.51822099157367,6.03212601064505E-17));
#14063=CARTESIAN_POINT('Ctrl Pts',(0.236649183304017,7.50653794848467,5.97068861804943E-17));
#14064=CARTESIAN_POINT('Ctrl Pts',(0.242860378108039,7.49433128865099,4.9439619065339E-17));
#14065=CARTESIAN_POINT('Ctrl Pts',(0.244940778165198,7.49024274584772,4.60006634751179E-17));
#14066=CARTESIAN_POINT('Ctrl Pts',(0.246919664339563,7.48609381169182,9.01432872076705E-17));
#14067=CARTESIAN_POINT('Ctrl Pts',(0.248793550657622,7.48189349080544,8.67361737988404E-17));
#14068=CARTESIAN_POINT('Ctrl Pts',(0.255493781437556,7.46687490669106,7.4553766620469E-17));
#14069=CARTESIAN_POINT('Ctrl Pts',(0.26081112509558,7.45130222640364,9.16174316001598E-17));
#14070=CARTESIAN_POINT('Ctrl Pts',(0.264722870572182,7.43540153025387,7.11236625150491E-17));
#14071=CARTESIAN_POINT('Ctrl Pts',(0.267427619696875,7.42440710481122,5.69533888287461E-17));
#14072=CARTESIAN_POINT('Ctrl Pts',(0.269459688552597,7.41325478922081,4.6972572244459E-17));
#14073=CARTESIAN_POINT('Ctrl Pts',(0.27079974443572,7.40201099931185,3.29597460435593E-17));
#14074=CARTESIAN_POINT('Ctrl Pts',(0.271554695341832,7.39567655498994,2.50653022589546E-17));
#14075=CARTESIAN_POINT('Ctrl Pts',(0.27208982123207,7.38931298403657,1.01541313543095E-16));
#14076=CARTESIAN_POINT('Ctrl Pts',(0.272400071186847,7.38293173498231,1.14491749414469E-16));
#14077=CARTESIAN_POINT('Ctrl Pts',(0.272610339929182,7.37860690852382,1.23268775233286E-16));
#14078=CARTESIAN_POINT('Ctrl Pts',(0.272716817601982,7.37428302936599,7.71694655557428E-17));
#14079=CARTESIAN_POINT('Ctrl Pts',(0.272719010540345,7.36996555954461,7.63278329429795E-17));
#14080=CARTESIAN_POINT('Ctrl Pts',(0.27272701832973,7.35419977716697,7.3254505933478E-17));
#14081=CARTESIAN_POINT('Ctrl Pts',(0.271347675050127,7.33851331166065,5.02512909736644E-18));
#14082=CARTESIAN_POINT('Ctrl Pts',(0.268538219226134,7.32308196703815,-6.93889390390723E-18));
#14083=CARTESIAN_POINT('Ctrl Pts',(0.266219736693056,7.31034736460601,-1.6812114944404E-17));
#14084=CARTESIAN_POINT('Ctrl Pts',(0.262926834287202,7.29778580690884,6.55929388800579E-17));
#14085=CARTESIAN_POINT('Ctrl Pts',(0.25873271504902,7.2854645892766,5.89805981832114E-17));
#14086=CARTESIAN_POINT('Ctrl Pts',(0.256787879633764,7.279751175077,5.59144206058319E-17));
#14087=CARTESIAN_POINT('Ctrl Pts',(0.254646960594001,7.27408549701033,9.6934502491867E-17));
#14088=CARTESIAN_POINT('Ctrl Pts',(0.252327976440821,7.26850105163772,9.71445146547012E-17));
#14089=CARTESIAN_POINT('Ctrl Pts',(0.245813541691288,7.25281336142979,9.77344757932954E-17));
#14090=CARTESIAN_POINT('Ctrl Pts',(0.237886985486038,7.23772772890658,5.31942244547902E-17));
#14091=CARTESIAN_POINT('Ctrl Pts',(0.228725953446014,7.22338664087012,2.42861286636753E-17));
#14092=CARTESIAN_POINT('Ctrl Pts',(0.223374596687987,7.21500938838961,7.3996541815834E-18));
#14093=CARTESIAN_POINT('Ctrl Pts',(0.217600970276322,7.20688618729852,1.2717535362053E-16));
#14094=CARTESIAN_POINT('Ctrl Pts',(0.211432869234838,7.19904719786575,1.35308431126191E-16));
#14095=CARTESIAN_POINT('Ctrl Pts',(0.207420256499723,7.19394760098548,1.40599344837786E-16));
#14096=CARTESIAN_POINT('Ctrl Pts',(0.203240590920077,7.18896831877402,8.31322120915072E-17));
#14097=CARTESIAN_POINT('Ctrl Pts',(0.198900453572221,7.18411827831884,8.32667268468867E-17));
#14098=CARTESIAN_POINT('Ctrl Pts',(0.195670954353016,7.18050935984282,8.33668193699228E-17));
#14099=CARTESIAN_POINT('Ctrl Pts',(0.192355312382397,7.17697524795826,4.32686351463275E-17));
#14100=CARTESIAN_POINT('Ctrl Pts',(0.188962380915405,7.17352497672425,3.81639164714898E-17));
#14101=CARTESIAN_POINT('Ctrl Pts',(0.17975235020419,7.16415929859711,2.43072806317295E-17));
#14102=CARTESIAN_POINT('Ctrl Pts',(0.169962167438026,7.15539778977274,5.97745424410255E-17));
#14103=CARTESIAN_POINT('Ctrl Pts',(0.159655188940229,7.14730762660204,4.5102810375397E-17));
#14104=CARTESIAN_POINT('Ctrl Pts',(0.154921336855726,7.14359192701095,3.83642875932839E-17));
#14105=CARTESIAN_POINT('Ctrl Pts',(0.150078290017851,7.14001794308044,6.33235573476612E-17));
#14106=CARTESIAN_POINT('Ctrl Pts',(0.145131356394006,7.13659282212682,6.24500451351651E-17));
#14107=CARTESIAN_POINT('Ctrl Pts',(0.139972270742195,7.13302081293665,6.15390718606404E-17));
#14108=CARTESIAN_POINT('Ctrl Pts',(0.134706655684311,7.12961533000732,6.44888900829108E-17));
#14109=CARTESIAN_POINT('Ctrl Pts',(0.129346139120924,7.12638655487346,6.24500451351651E-17));
#14110=CARTESIAN_POINT('Ctrl Pts',(0.117404508126543,7.11919380754091,5.79081071087007E-17));
#14111=CARTESIAN_POINT('Ctrl Pts',(0.104985462890608,7.11287199690184,1.81867207105765E-17));
#14112=CARTESIAN_POINT('Ctrl Pts',(0.0921567668402144,7.10750685206111,
-6.93889390390723E-18));
#14113=CARTESIAN_POINT('Ctrl Pts',(0.0880066571319542,7.10577121660741,
-2.89761322741409E-17));
#14114=CARTESIAN_POINT('Ctrl Pts',(0.0838135816987372,7.10413581036214,
-6.25245253825226E-20));
#14115=CARTESIAN_POINT('Ctrl Pts',(0.0795808873001328,7.10259971193733,
0.));
#14116=CARTESIAN_POINT('Ctrl Pts',(-0.251664502419995,7.39978648873079,
-0.161258330249198));
#14117=CARTESIAN_POINT('Ctrl Pts',(-0.251853743060092,7.37731968999655,
-0.15983892928355));
#14118=CARTESIAN_POINT('Ctrl Pts',(-0.249087060170416,7.35489869942726,
-0.158419528317902));
#14119=CARTESIAN_POINT('Ctrl Pts',(-0.243177144710154,7.33333937551853,
-0.157000127352253));
#14120=CARTESIAN_POINT('Ctrl Pts',(-0.221387260518207,7.25385005382068,
-0.151766789773845));
#14121=CARTESIAN_POINT('Ctrl Pts',(-0.156868268663584,7.18607422982997,
-0.146533452195437));
#14122=CARTESIAN_POINT('Ctrl Pts',(-0.0785474512786524,7.16039843377808,
-0.141300114617028));
#14123=CARTESIAN_POINT('Ctrl Pts',(-0.00022663389372081,7.13472263772619,
-0.13606677703862));
#14124=CARTESIAN_POINT('Ctrl Pts',(0.0918960090215198,7.15114686961312,
-0.130833439460211));
#14125=CARTESIAN_POINT('Ctrl Pts',(0.156516611947103,7.20230943571013,-0.125600101881803));
#14126=CARTESIAN_POINT('Ctrl Pts',(0.221137214872687,7.25347200180715,-0.120366764303394));
#14127=CARTESIAN_POINT('Ctrl Pts',(0.258255777808613,7.33937290211427,-0.115133426724986));
#14128=CARTESIAN_POINT('Ctrl Pts',(0.251230492354282,7.42149364017549,-0.109900089146577));
#14129=CARTESIAN_POINT('Ctrl Pts',(0.244205206899952,7.50361437823672,-0.104666751568169));
#14130=CARTESIAN_POINT('Ctrl Pts',(0.193036073055365,7.58195495405205,-0.0994334139897605));
#14131=CARTESIAN_POINT('Ctrl Pts',(0.120664054720216,7.62139990068305,-0.0942000764113521));
#14132=CARTESIAN_POINT('Ctrl Pts',(0.0482920363850678,7.66084484731404,
-0.0889667388329436));
#14133=CARTESIAN_POINT('Ctrl Pts',(-0.0452828664406417,7.66139416476069,
-0.0837334012545352));
#14134=CARTESIAN_POINT('Ctrl Pts',(-0.118103955917399,7.6227836008624,-0.0785000636761267));
#14135=CARTESIAN_POINT('Ctrl Pts',(-0.190925045394156,7.5841730369641,-0.0732667260977183));
#14136=CARTESIAN_POINT('Ctrl Pts',(-0.242992321521962,7.50640259172086,
-0.0680333885193098));
#14137=CARTESIAN_POINT('Ctrl Pts',(-0.25096508216279,7.42437725852632,-0.0628000509409014));
#14138=CARTESIAN_POINT('Ctrl Pts',(-0.251747996817527,7.41632247821737,
-0.0622861440436668));
#14139=CARTESIAN_POINT('Ctrl Pts',(-0.252105708816997,7.40822666809701,
-0.0617722371464322));
#14140=CARTESIAN_POINT('Ctrl Pts',(-0.252053546614158,7.40012638988493,
-0.0612583302491975));
#14141=CARTESIAN_POINT('Ctrl Pts',(-0.0793799282532879,7.10307770462543,
5.55111512312578E-17));
#14142=CARTESIAN_POINT('Ctrl Pts',(-0.177014005842308,7.12917943627315,
-0.00523333757840839));
#14143=CARTESIAN_POINT('Ctrl Pts',(-0.342929363773459,7.28476228830982,
-0.0157000127352253));
#14144=CARTESIAN_POINT('Ctrl Pts',(-0.285303662486741,7.6230159413608,-0.0314000254704506));
#14145=CARTESIAN_POINT('Ctrl Pts',(0.0286357548570192,7.76072194419717,
-0.047100038205676));
#14146=CARTESIAN_POINT('Ctrl Pts',(0.316662279094702,7.57523911945597,-0.0628000509409012));
#14147=CARTESIAN_POINT('Ctrl Pts',(0.320851004579023,7.23248257807725,-0.0785000636761267));
#14148=CARTESIAN_POINT('Ctrl Pts',(0.037271918951097,7.04000744673753,-0.094200076411352));
#14149=CARTESIAN_POINT('Ctrl Pts',(-0.279700685926573,7.17030791937543,
-0.109900089146577));
#14150=CARTESIAN_POINT('Ctrl Pts',(-0.345877162555279,7.50659192636033,
-0.125600101881803));
#14151=CARTESIAN_POINT('Ctrl Pts',(-0.101895250628719,7.74728578061798,
-0.141300114617028));
#14152=CARTESIAN_POINT('Ctrl Pts',(0.233453631148172,7.67656918324398,-0.157000127352253));
#14153=CARTESIAN_POINT('Ctrl Pts',(0.359464126606772,7.35784834370038,-0.172700140087479));
#14154=CARTESIAN_POINT('Ctrl Pts',(0.163138836475842,7.07692629120202,-0.188400152822704));
#14155=CARTESIAN_POINT('Ctrl Pts',(-0.179474189751402,7.08570704088486,
-0.20410016555793));
#14156=CARTESIAN_POINT('Ctrl Pts',(-0.361151198222271,7.37631754602761,
-0.219800178293155));
#14157=CARTESIAN_POINT('Ctrl Pts',(-0.218980358434117,7.68816421398779,
-0.23550019102838));
#14158=CARTESIAN_POINT('Ctrl Pts',(0.119552217972776,7.7416113266484,-0.251200203763606));
#14159=CARTESIAN_POINT('Ctrl Pts',(0.350881199163606,7.48873225573956,-0.266900216498831));
#14160=CARTESIAN_POINT('Ctrl Pts',(0.267571630187383,7.15628613456826,-0.282600229234056));
#14161=CARTESIAN_POINT('Ctrl Pts',(-0.0556719802611724,7.04238056731933,
-0.298300241969282));
#14162=CARTESIAN_POINT('Ctrl Pts',(-0.328993995030839,7.24915577981674,
-0.314000254704507));
#14163=CARTESIAN_POINT('Ctrl Pts',(-0.307303936687348,7.59119444989383,
-0.329700267439732));
#14164=CARTESIAN_POINT('Ctrl Pts',(-0.0100514909408711,7.76178722340353,
-0.345400280174958));
#14165=CARTESIAN_POINT('Ctrl Pts',(0.296214223541038,7.60796192241644,-0.361100292910183));
#14166=CARTESIAN_POINT('Ctrl Pts',(0.336861801835373,7.26765517072256,-0.376800305645408));
#14167=CARTESIAN_POINT('Ctrl Pts',(0.0754421708108413,7.04602329698811,
-0.392500318380633));
#14168=CARTESIAN_POINT('Ctrl Pts',(-0.253627178584431,7.14180572880535,
-0.408200331115859));
#14169=CARTESIAN_POINT('Ctrl Pts',(-0.355266603733067,7.46911344056264,
-0.423900343851084));
#14170=CARTESIAN_POINT('Ctrl Pts',(-0.138335057048331,7.73444646717113,
-0.43960035658631));
#14171=CARTESIAN_POINT('Ctrl Pts',(0.202642862416027,7.69987813805627,-0.455300369321535));
#14172=CARTESIAN_POINT('Ctrl Pts',(0.361908983097054,7.39640620579093,-0.47100038205676));
#14173=CARTESIAN_POINT('Ctrl Pts',(0.196647846607491,7.09615686298222,-0.486700394791986));
#14174=CARTESIAN_POINT('Ctrl Pts',(-0.144949300426615,7.06836657665492,
-0.502400407527211));
#14175=CARTESIAN_POINT('Ctrl Pts',(-0.356569019314508,7.33795516142226,
-0.518100420262437));
#14176=CARTESIAN_POINT('Ctrl Pts',(-0.248449877558159,7.66317995052507,
-0.533800432997661));
#14177=CARTESIAN_POINT('Ctrl Pts',(0.0824566524067525,7.75240874841395,
-0.549500445732887));
#14178=CARTESIAN_POINT('Ctrl Pts',(0.339423512150486,7.52562925031437,-0.565200458468112));
#14179=CARTESIAN_POINT('Ctrl Pts',(0.292026050158285,7.1861967789166,-0.580900471203337));
#14180=CARTESIAN_POINT('Ctrl Pts',(-0.0172339683272763,7.03848374595487,
-0.596600483938563));
#14181=CARTESIAN_POINT('Ctrl Pts',(-0.311040130662272,7.21494572763339,
-0.612300496673788));
#14182=CARTESIAN_POINT('Ctrl Pts',(-0.325933606530968,7.55734780923163,
-0.628000509409014));
#14183=CARTESIAN_POINT('Ctrl Pts',(-0.0485593254958618,7.75865428087583,
-0.643700522144239));
#14184=CARTESIAN_POINT('Ctrl Pts',(0.27235863905538,7.63835266345873,-0.659400534879465));
#14185=CARTESIAN_POINT('Ctrl Pts',(0.349049856868627,7.30431662403272,-0.67510054761469));
#14186=CARTESIAN_POINT('Ctrl Pts',(0.112745006295209,7.05608341261925,-0.690800560349915));
#14187=CARTESIAN_POINT('Ctrl Pts',(-0.224659951867446,7.11623820488055,
-0.70650057308514));
#14188=CARTESIAN_POINT('Ctrl Pts',(-0.360609008143163,7.4308556130298,-0.722200585820366));
#14189=CARTESIAN_POINT('Ctrl Pts',(-0.173198863217152,7.71778292610997,
-0.73790059855559));
#14190=CARTESIAN_POINT('Ctrl Pts',(0.169525116851479,7.71979476003134,-0.753600611290817));
#14191=CARTESIAN_POINT('Ctrl Pts',(0.360224711692468,7.43495575882791,-0.769300624026041));
#14192=CARTESIAN_POINT('Ctrl Pts',(0.227926662850033,7.11894882344372,-0.785000636761268));
#14193=CARTESIAN_POINT('Ctrl Pts',(-0.108793818048451,7.05460429203039,
-0.800700649496493));
#14194=CARTESIAN_POINT('Ctrl Pts',(-0.34788417951995,7.30071819716892,-0.816400662231718));
#14195=CARTESIAN_POINT('Ctrl Pts',(-0.29928159504458,7.52291567381437,-0.826867337388535));
#14196=CARTESIAN_POINT('Ctrl Pts',(-0.233606265769613,7.59973015569307,
-0.832100674966943));
#14197=CARTESIAN_POINT('Ctrl Pts',(-0.0745932854346959,7.12098224301579,
0.0107002249889811));
#14198=CARTESIAN_POINT('Ctrl Pts',(-0.166339987378199,7.14551002934643,
0.00546688741057267));
#14199=CARTESIAN_POINT('Ctrl Pts',(-0.322250579948499,7.291711170442,-0.00499978774624421));
#14200=CARTESIAN_POINT('Ctrl Pts',(-0.268099732510858,7.60956798697692,
-0.0206998004814696));
#14201=CARTESIAN_POINT('Ctrl Pts',(0.026909006882343,7.73897026034341,-0.0363998132166949));
#14202=CARTESIAN_POINT('Ctrl Pts',(0.297567411443636,7.56467212738206,-0.0520998259519203));
#14203=CARTESIAN_POINT('Ctrl Pts',(0.301503555032259,7.24258394856573,-0.0677998386871455));
#14204=CARTESIAN_POINT('Ctrl Pts',(0.0350244066755359,7.06171514801338,
-0.083499851422371));
#14205=CARTESIAN_POINT('Ctrl Pts',(-0.262834617776779,7.18415844774452,
-0.0991998641575963));
#14206=CARTESIAN_POINT('Ctrl Pts',(-0.325020625232928,7.50016438869357,
-0.114899876892822));
#14207=CARTESIAN_POINT('Ctrl Pts',(-0.0957509244696644,7.72634430303828,
-0.130599889628047));
#14208=CARTESIAN_POINT('Ctrl Pts',(0.219376279711874,7.6598919460135,-0.146299902363272));
#14209=CARTESIAN_POINT('Ctrl Pts',(0.337788289678909,7.36039010617557,-0.161999915098498));
#14210=CARTESIAN_POINT('Ctrl Pts',(0.153301496518078,7.09640777074127,-0.177699927833723));
#14211=CARTESIAN_POINT('Ctrl Pts',(-0.168651821170329,7.10465903755185,
-0.193399940568948));
#14212=CARTESIAN_POINT('Ctrl Pts',(-0.33937363017156,7.3777456078907,-0.209099953304174));
#14213=CARTESIAN_POINT('Ctrl Pts',(-0.20577575138576,7.67078779156197,-0.224799966039399));
#14214=CARTESIAN_POINT('Ctrl Pts',(0.112343169310245,7.72101202101242,-0.240499978774624));
#14215=CARTESIAN_POINT('Ctrl Pts',(0.329722916344349,7.48338166366851,-0.25619999150985));
#14216=CARTESIAN_POINT('Ctrl Pts',(0.251436949163123,7.17098218241599,-0.271900004245075));
#14217=CARTESIAN_POINT('Ctrl Pts',(-0.052314936605708,7.06394516843321,
-0.287600016980301));
#14218=CARTESIAN_POINT('Ctrl Pts',(-0.309155519759742,7.25825174927847,
-0.303300029715525));
#14219=CARTESIAN_POINT('Ctrl Pts',(-0.288773380991002,7.5796653447324,-0.319000042450752));
#14220=CARTESIAN_POINT('Ctrl Pts',(-0.00944538184015792,7.73997130276882,
-0.334700055185976));
#14221=CARTESIAN_POINT('Ctrl Pts',(0.278352382177899,7.59542173166067,-0.350400067921202));
#14222=CARTESIAN_POINT('Ctrl Pts',(0.316548894528777,7.27563561918828,-0.366100080656427));
#14223=CARTESIAN_POINT('Ctrl Pts',(0.0708929764102307,7.06736823998195,
-0.381800093391652));
#14224=CARTESIAN_POINT('Ctrl Pts',(-0.238333353814305,7.15737495116686,
-0.397500106126878));
#14225=CARTESIAN_POINT('Ctrl Pts',(-0.333843879187155,7.46494587123854,
-0.413200118862103));
#14226=CARTESIAN_POINT('Ctrl Pts',(-0.12999339534681,7.71427920555331,-0.428900131597329));
#14227=CARTESIAN_POINT('Ctrl Pts',(0.190423413199248,7.68179536111799,-0.444600144332554));
#14228=CARTESIAN_POINT('Ctrl Pts',(0.340085720301983,7.39662291308232,-0.460300157067779));
#14229=CARTESIAN_POINT('Ctrl Pts',(0.184789899347173,7.11447873101343,-0.476000169803005));
#14230=CARTESIAN_POINT('Ctrl Pts',(-0.136208797087621,7.08836421055545,
-0.49170018253823));
#14231=CARTESIAN_POINT('Ctrl Pts',(-0.335067758565214,7.34169649109518,
-0.507400195273455));
#14232=CARTESIAN_POINT('Ctrl Pts',(-0.233468246201688,7.64731008961818,
-0.523100208008681));
#14233=CARTESIAN_POINT('Ctrl Pts',(0.0774844818370269,7.73115835373707,
-0.538800220743906));
#14234=CARTESIAN_POINT('Ctrl Pts',(0.318956132642252,7.51805375406419,-0.554500233479132));
#14235=CARTESIAN_POINT('Ctrl Pts',(0.274416757398889,7.199089202421,-0.570200246214356));
#14236=CARTESIAN_POINT('Ctrl Pts',(-0.016194752841135,7.06028332702413,
-0.585900258949582));
#14237=CARTESIAN_POINT('Ctrl Pts',(-0.292284280909198,7.22610457752611,
-0.601600271684807));
#14238=CARTESIAN_POINT('Ctrl Pts',(-0.306279673964272,7.54785967063472,
-0.617300284420033));
#14239=CARTESIAN_POINT('Ctrl Pts',(-0.0456311778926191,7.7370272779837,
-0.633000297155258));
#14240=CARTESIAN_POINT('Ctrl Pts',(0.255935299397576,7.62397989832853,-0.648700309890484));
#14241=CARTESIAN_POINT('Ctrl Pts',(0.328002004754429,7.31008637155593,-0.664400322625709));
#14242=CARTESIAN_POINT('Ctrl Pts',(0.105946435339172,7.07682172643994,-0.680100335360934));
#14243=CARTESIAN_POINT('Ctrl Pts',(-0.211112862963559,7.13334915961038,
-0.695800348096159));
#14244=CARTESIAN_POINT('Ctrl Pts',(-0.338864134380612,7.42899500668041,
-0.711500360831385));
#14245=CARTESIAN_POINT('Ctrl Pts',(-0.162754899446344,7.69862048297595,
-0.72720037356661));
#14246=CARTESIAN_POINT('Ctrl Pts',(0.159302681520486,7.70051100247185,-0.742900386301834));
#14247=CARTESIAN_POINT('Ctrl Pts',(0.338503011166357,7.43284791197487,-0.758600399037062));
#14248=CARTESIAN_POINT('Ctrl Pts',(0.214182589909887,7.13589632674239,-0.774300411772284));
#14249=CARTESIAN_POINT('Ctrl Pts',(-0.102233505393505,7.07543179744019,
-0.790000424507513));
#14250=CARTESIAN_POINT('Ctrl Pts',(-0.326906618236604,7.30670493133454,
-0.805700437242736));
#14251=CARTESIAN_POINT('Ctrl Pts',(-0.281234789899004,7.51550380736019,
-0.816167112399554));
#14252=CARTESIAN_POINT('Ctrl Pts',(-0.21951971040191,7.58768634390788,-0.821400449977962));
#14253=CARTESIAN_POINT('Ctrl Pts',(-0.0698066426161039,7.13888678140614,
0.0214004499779622));
#14254=CARTESIAN_POINT('Ctrl Pts',(-0.155665968914089,7.1618406224197,0.0161671123995537));
#14255=CARTESIAN_POINT('Ctrl Pts',(-0.301571796123539,7.29866005257418,
0.00570043724273684));
#14256=CARTESIAN_POINT('Ctrl Pts',(-0.250895802534975,7.59612003259303,
-0.00999957549248849));
#14257=CARTESIAN_POINT('Ctrl Pts',(0.0251822589076668,7.71721857648964,
-0.0256995882277138));
#14258=CARTESIAN_POINT('Ctrl Pts',(0.27847254379257,7.55410513530815,-0.0413996009629392));
#14259=CARTESIAN_POINT('Ctrl Pts',(0.282156105485495,7.25268531905421,-0.0570996136981645));
#14260=CARTESIAN_POINT('Ctrl Pts',(0.0327768943999749,7.08342284928922,
-0.0727996264333899));
#14261=CARTESIAN_POINT('Ctrl Pts',(-0.245968549626985,7.19800897611362,
-0.0884996391686152));
#14262=CARTESIAN_POINT('Ctrl Pts',(-0.304164087910577,7.49373685102681,
-0.104199651903841));
#14263=CARTESIAN_POINT('Ctrl Pts',(-0.089606598310609,7.70540282545859,
-0.119899664639066));
#14264=CARTESIAN_POINT('Ctrl Pts',(0.205298928275576,7.64321470878302,-0.135599677374291));
#14265=CARTESIAN_POINT('Ctrl Pts',(0.316112452751045,7.36293186865078,-0.151299690109517));
#14266=CARTESIAN_POINT('Ctrl Pts',(0.143464156560313,7.11588925028052,-0.166999702844742));
#14267=CARTESIAN_POINT('Ctrl Pts',(-0.157829452589257,7.12361103421885,
-0.182699715579967));
#14268=CARTESIAN_POINT('Ctrl Pts',(-0.317596062120848,7.3791736697538,-0.198399728315193));
#14269=CARTESIAN_POINT('Ctrl Pts',(-0.192571144337404,7.65341136913615,
-0.214099741050418));
#14270=CARTESIAN_POINT('Ctrl Pts',(0.105134120647715,7.70041271537645,-0.229799753785644));
#14271=CARTESIAN_POINT('Ctrl Pts',(0.308564633525091,7.47803107159744,-0.245499766520869));
#14272=CARTESIAN_POINT('Ctrl Pts',(0.235302268138864,7.18567823026373,-0.261199779256094));
#14273=CARTESIAN_POINT('Ctrl Pts',(-0.0489578929502435,7.08550976954708,
-0.276899791991319));
#14274=CARTESIAN_POINT('Ctrl Pts',(-0.289317044488645,7.26734771874021,
-0.292599804726545));
#14275=CARTESIAN_POINT('Ctrl Pts',(-0.270242825294655,7.56813623957097,
-0.30829981746177));
#14276=CARTESIAN_POINT('Ctrl Pts',(-0.00883927273944482,7.71815538213412,
-0.323999830196996));
#14277=CARTESIAN_POINT('Ctrl Pts',(0.260490540814761,7.5828815409049,-0.33969984293222));
#14278=CARTESIAN_POINT('Ctrl Pts',(0.296235987222181,7.28361606765402,-0.355399855667446));
#14279=CARTESIAN_POINT('Ctrl Pts',(0.0663437820096206,7.08871318297577,
-0.371099868402671));
#14280=CARTESIAN_POINT('Ctrl Pts',(-0.22303952904418,7.17294417352836,-0.386799881137897));
#14281=CARTESIAN_POINT('Ctrl Pts',(-0.312421154641242,7.46077830191444,
-0.402499893873122));
#14282=CARTESIAN_POINT('Ctrl Pts',(-0.12165173364529,7.69411194393548,-0.418199906608348));
#14283=CARTESIAN_POINT('Ctrl Pts',(0.178203963982469,7.66371258417972,-0.433899919343573));
#14284=CARTESIAN_POINT('Ctrl Pts',(0.31826245750691,7.39683962037371,-0.449599932078798));
#14285=CARTESIAN_POINT('Ctrl Pts',(0.172931952086855,7.13280059904465,-0.465299944814023));
#14286=CARTESIAN_POINT('Ctrl Pts',(-0.127468293748627,7.108361844456,-0.480999957549249));
#14287=CARTESIAN_POINT('Ctrl Pts',(-0.31356649781592,7.3454378207681,-0.496699970284474));
#14288=CARTESIAN_POINT('Ctrl Pts',(-0.218486614845218,7.63144022871131,
-0.512399983019699));
#14289=CARTESIAN_POINT('Ctrl Pts',(0.0725123112673016,7.70990795906018,
-0.528099995754925));
#14290=CARTESIAN_POINT('Ctrl Pts',(0.298488753134019,7.51047825781402,-0.54380000849015));
#14291=CARTESIAN_POINT('Ctrl Pts',(0.256807464639494,7.2119816259254,-0.559500021225375));
#14292=CARTESIAN_POINT('Ctrl Pts',(-0.0151555373549939,7.08208290809339,
-0.575200033960601));
#14293=CARTESIAN_POINT('Ctrl Pts',(-0.273528431156123,7.23726342741883,
-0.590900046695826));
#14294=CARTESIAN_POINT('Ctrl Pts',(-0.286625741397577,7.53837153203782,
-0.606600059431052));
#14295=CARTESIAN_POINT('Ctrl Pts',(-0.0427030302893763,7.71540027509155,
-0.622300072166277));
#14296=CARTESIAN_POINT('Ctrl Pts',(0.23951195973977,7.60960713319833,-0.638000084901503));
#14297=CARTESIAN_POINT('Ctrl Pts',(0.306954152640232,7.31585611907914,-0.653700097636727));
#14298=CARTESIAN_POINT('Ctrl Pts',(0.0991478643831351,7.09756004026064,
-0.669400110371954));
#14299=CARTESIAN_POINT('Ctrl Pts',(-0.19756577405967,7.15046011434021,-0.685100123107178));
#14300=CARTESIAN_POINT('Ctrl Pts',(-0.317119260618062,7.42713440033102,
-0.700800135842404));
#14301=CARTESIAN_POINT('Ctrl Pts',(-0.152310935675535,7.67945803984195,
-0.716500148577629));
#14302=CARTESIAN_POINT('Ctrl Pts',(0.149080246189493,7.68122724491234,-0.732200161312854));
#14303=CARTESIAN_POINT('Ctrl Pts',(0.316781310640245,7.43074006512186,-0.74790017404808));
#14304=CARTESIAN_POINT('Ctrl Pts',(0.20043851696974,7.15284383004104,-0.763600186783305));
#14305=CARTESIAN_POINT('Ctrl Pts',(-0.0956731927385576,7.09625930285,-0.779300199518531));
#14306=CARTESIAN_POINT('Ctrl Pts',(-0.305929056953258,7.31269166550016,
-0.795000212253756));
#14307=CARTESIAN_POINT('Ctrl Pts',(-0.263187984753428,7.508091940906,-0.805466887410573));
#14308=CARTESIAN_POINT('Ctrl Pts',(-0.205433155034207,7.57564253212269,
-0.810700224988981));
#14309=CARTESIAN_POINT('Ctrl Pts',(-0.065019999797512,7.15679131979649,
0.0321006749669432));
#14310=CARTESIAN_POINT('Ctrl Pts',(-0.14499195044998,7.17817121549298,0.0268673373885348));
#14311=CARTESIAN_POINT('Ctrl Pts',(-0.280893012298579,7.30560893470636,
0.0164006622317179));
#14312=CARTESIAN_POINT('Ctrl Pts',(-0.233691872559092,7.58267207820915,
0.000700649496492578));
#14313=CARTESIAN_POINT('Ctrl Pts',(0.0234555109329906,7.69546689263588,
-0.0149993632387328));
#14314=CARTESIAN_POINT('Ctrl Pts',(0.259377676141504,7.54353814323423,-0.0306993759739581));
#14315=CARTESIAN_POINT('Ctrl Pts',(0.262808655938731,7.26278668954269,-0.0463993887091835));
#14316=CARTESIAN_POINT('Ctrl Pts',(0.0305293821244139,7.10513055056507,
-0.0620994014444087));
#14317=CARTESIAN_POINT('Ctrl Pts',(-0.229102481477192,7.21185950448272,
-0.0777994141796342));
#14318=CARTESIAN_POINT('Ctrl Pts',(-0.283307550588226,7.48730931336005,
-0.0934994269148594));
#14319=CARTESIAN_POINT('Ctrl Pts',(-0.083462272151554,7.68446134787889,
-0.109199439650085));
#14320=CARTESIAN_POINT('Ctrl Pts',(0.191221576839279,7.62653747155253,-0.12489945238531));
#14321=CARTESIAN_POINT('Ctrl Pts',(0.294436615823181,7.36547363112598,-0.140599465120536));
#14322=CARTESIAN_POINT('Ctrl Pts',(0.133626816602548,7.13537072981977,-0.156299477855761));
#14323=CARTESIAN_POINT('Ctrl Pts',(-0.147007084008184,7.14256303088585,
-0.171999490590986));
#14324=CARTESIAN_POINT('Ctrl Pts',(-0.295818494070137,7.38060173161688,
-0.187699503326212));
#14325=CARTESIAN_POINT('Ctrl Pts',(-0.179366537289048,7.63603494671035,
-0.203399516061437));
#14326=CARTESIAN_POINT('Ctrl Pts',(0.0979250719851847,7.67981340974047,
-0.219099528796663));
#14327=CARTESIAN_POINT('Ctrl Pts',(0.287406350705833,7.47268047952639,-0.234799541531887));
#14328=CARTESIAN_POINT('Ctrl Pts',(0.219167587114604,7.20037427811147,-0.250499554267113));
#14329=CARTESIAN_POINT('Ctrl Pts',(-0.045600849294779,7.10707437066095,
-0.266199567002338));
#14330=CARTESIAN_POINT('Ctrl Pts',(-0.269478569217549,7.27644368820193,
-0.281899579737564));
#14331=CARTESIAN_POINT('Ctrl Pts',(-0.251712269598308,7.55660713440954,
-0.297599592472789));
#14332=CARTESIAN_POINT('Ctrl Pts',(-0.00823316363873174,7.6963394614994,
-0.313299605208015));
#14333=CARTESIAN_POINT('Ctrl Pts',(0.242628699451623,7.57034135014914,-0.328999617943239));
#14334=CARTESIAN_POINT('Ctrl Pts',(0.275923079915585,7.29159651611974,-0.344699630678465));
#14335=CARTESIAN_POINT('Ctrl Pts',(0.0617945876090101,7.11005812596961,
-0.36039964341369));
#14336=CARTESIAN_POINT('Ctrl Pts',(-0.207745704274054,7.18851339588986,
-0.376099656148916));
#14337=CARTESIAN_POINT('Ctrl Pts',(-0.290998430095329,7.45661073259035,
-0.391799668884141));
#14338=CARTESIAN_POINT('Ctrl Pts',(-0.113310071943769,7.67394468231766,
-0.407499681619367));
#14339=CARTESIAN_POINT('Ctrl Pts',(0.16598451476569,7.64562980724146,-0.423199694354591));
#14340=CARTESIAN_POINT('Ctrl Pts',(0.296439194711838,7.39705632766509,-0.438899707089818));
#14341=CARTESIAN_POINT('Ctrl Pts',(0.161074004826536,7.15112246707589,-0.454599719825042));
#14342=CARTESIAN_POINT('Ctrl Pts',(-0.118727790409632,7.12835947835651,
-0.470299732560268));
#14343=CARTESIAN_POINT('Ctrl Pts',(-0.292065237066626,7.34917915044104,
-0.485999745295493));
#14344=CARTESIAN_POINT('Ctrl Pts',(-0.203504983488747,7.61557036780441,
-0.501699758030719));
#14345=CARTESIAN_POINT('Ctrl Pts',(0.0675401406975761,7.68865756438332,
-0.517399770765944));
#14346=CARTESIAN_POINT('Ctrl Pts',(0.278021373625785,7.50290276156383,-0.533099783501169));
#14347=CARTESIAN_POINT('Ctrl Pts',(0.239198171880098,7.22487404942981,-0.548799796236395));
#14348=CARTESIAN_POINT('Ctrl Pts',(-0.0141163218688527,7.10388248916265,
-0.56449980897162));
#14349=CARTESIAN_POINT('Ctrl Pts',(-0.254772581403049,7.24842227731155,
-0.580199821706845));
#14350=CARTESIAN_POINT('Ctrl Pts',(-0.266971808830881,7.52888339344091,
-0.595899834442071));
#14351=CARTESIAN_POINT('Ctrl Pts',(-0.0397748826861335,7.69377327219942,
-0.611599847177295));
#14352=CARTESIAN_POINT('Ctrl Pts',(0.223088620081966,7.59523436806812,-0.627299859912522));
#14353=CARTESIAN_POINT('Ctrl Pts',(0.285906300526035,7.32162586660236,-0.642999872647746));
#14354=CARTESIAN_POINT('Ctrl Pts',(0.0923492934270986,7.11829835408133,
-0.658699885382973));
#14355=CARTESIAN_POINT('Ctrl Pts',(-0.184018685155783,7.16757106907005,
-0.674399898118197));
#14356=CARTESIAN_POINT('Ctrl Pts',(-0.295374386855511,7.42527379398162,
-0.690099910853423));
#14357=CARTESIAN_POINT('Ctrl Pts',(-0.141866971904727,7.66029559670794,
-0.705799923588648));
#14358=CARTESIAN_POINT('Ctrl Pts',(0.1388578108585,7.66194348735283,-0.721499936323873));
#14359=CARTESIAN_POINT('Ctrl Pts',(0.295059610114134,7.42863221826883,-0.737199949059098));
#14360=CARTESIAN_POINT('Ctrl Pts',(0.186694444029594,7.1697913333397,-0.752899961794324));
#14361=CARTESIAN_POINT('Ctrl Pts',(-0.0891128800836106,7.11708680825981,
-0.76859997452955));
#14362=CARTESIAN_POINT('Ctrl Pts',(-0.284951495669912,7.31867839966577,
-0.784299987264775));
#14363=CARTESIAN_POINT('Ctrl Pts',(-0.245141179607851,7.50068007445182,
-0.794766662421592));
#14364=CARTESIAN_POINT('Ctrl Pts',(-0.191346599666504,7.5635987203375,-0.8));
#14365=CARTESIAN_POINT('Ctrl Pts',(-0.25159361924534,7.40020120251426,-0.088741669750802));
#14366=CARTESIAN_POINT('Ctrl Pts',(-0.251789088068147,7.4253219403653,-0.0903275888054879));
#14367=CARTESIAN_POINT('Ctrl Pts',(-0.248321666625649,7.45039001357577,
-0.0919135078601738));
#14368=CARTESIAN_POINT('Ctrl Pts',(-0.240965825996942,7.4742596843003,-0.0934994269148597));
#14369=CARTESIAN_POINT('Ctrl Pts',(-0.216692457776002,7.55302665819966,
-0.0987327644932681));
#14370=CARTESIAN_POINT('Ctrl Pts',(-0.150077364963778,7.61874400303928,
-0.103966102071677));
#14371=CARTESIAN_POINT('Ctrl Pts',(-0.070989177059194,7.64194869607136,
-0.109199439650085));
#14372=CARTESIAN_POINT('Ctrl Pts',(0.00809901084539029,7.66515338910344,
-0.114432777228493));
#14373=CARTESIAN_POINT('Ctrl Pts',(0.0996602938423346,7.64584543032799,
-0.119666114806902));
#14374=CARTESIAN_POINT('Ctrl Pts',(0.162643441838124,7.59268081086917,-0.12489945238531));
#14375=CARTESIAN_POINT('Ctrl Pts',(0.225626589833913,7.53951619141035,-0.130132789963719));
#14376=CARTESIAN_POINT('Ctrl Pts',(0.260031602828547,7.45249491126816,-0.135366127542127));
#14377=CARTESIAN_POINT('Ctrl Pts',(0.250432476122426,7.37063378764604,-0.140599465120536));
#14378=CARTESIAN_POINT('Ctrl Pts',(0.240833349416304,7.28877266402391,-0.145832802698944));
#14379=CARTESIAN_POINT('Ctrl Pts',(0.187230083009426,7.21207169692184,-0.151066140277353));
#14380=CARTESIAN_POINT('Ctrl Pts',(0.113656133037532,7.17491993021515,-0.156299477855761));
#14381=CARTESIAN_POINT('Ctrl Pts',(0.0400821830656374,7.13776816350846,
-0.161532815434169));
#14382=CARTESIAN_POINT('Ctrl Pts',(-0.0534624504712735,7.14016559719716,
-0.166766153012578));
#14383=CARTESIAN_POINT('Ctrl Pts',(-0.125036668916721,7.18103743083001,
-0.171999490590986));
#14384=CARTESIAN_POINT('Ctrl Pts',(-0.196610887362169,7.22190926446286,
-0.177232828169395));
#14385=CARTESIAN_POINT('Ctrl Pts',(-0.246214690716153,7.30125549803987,
-0.182466165747803));
#14386=CARTESIAN_POINT('Ctrl Pts',(-0.25160793292963,7.38350081734395,-0.187699503326212));
#14387=CARTESIAN_POINT('Ctrl Pts',(-0.251965936203217,7.38896025943511,
-0.188046892134409));
#14388=CARTESIAN_POINT('Ctrl Pts',(-0.252129134444029,7.39443247577015,
-0.188394280942605));
#14389=CARTESIAN_POINT('Ctrl Pts',(-0.252102618136395,7.39990630057405,
-0.188741669750802));
#14390=CARTESIAN_POINT('Ctrl Pts',(-0.0793799282532879,7.10307770462543,
5.55111512312578E-17));
#14391=CARTESIAN_POINT('Ctrl Pts',(-0.0961911438687228,7.10922732239277,
6.3088022331286E-17));
#14392=CARTESIAN_POINT('Ctrl Pts',(-0.112330824293046,7.11692875641727,
7.51298486027343E-17));
#14393=CARTESIAN_POINT('Ctrl Pts',(-0.127669362876862,7.1259997700432,8.37004077158809E-17));
#14394=CARTESIAN_POINT('Ctrl Pts',(-0.137645054815231,7.13189926542253,
8.92744235835032E-17));
#14395=CARTESIAN_POINT('Ctrl Pts',(-0.147281435088536,7.1383791577173,7.60600198292336E-17));
#14396=CARTESIAN_POINT('Ctrl Pts',(-0.156535227934782,7.14539793713334,
8.06646416329215E-17));
#14397=CARTESIAN_POINT('Ctrl Pts',(-0.16394892482158,7.15102104799938,8.43536447150178E-17));
#14398=CARTESIAN_POINT('Ctrl Pts',(-0.171116962103292,7.15699019329351,
4.93210431432864E-17));
#14399=CARTESIAN_POINT('Ctrl Pts',(-0.178013423245633,7.16328599091072,
3.46944695195361E-17));
#14400=CARTESIAN_POINT('Ctrl Pts',(-0.181540425610593,7.16650580069822,
2.72141171043684E-17));
#14401=CARTESIAN_POINT('Ctrl Pts',(-0.184990066957579,7.16980542739394,
7.26266936595826E-17));
#14402=CARTESIAN_POINT('Ctrl Pts',(-0.188356628917223,7.17317858145051,
7.28583859910259E-17));
#14403=CARTESIAN_POINT('Ctrl Pts',(-0.200715855331018,7.18556200858287,
7.37089682814972E-17));
#14404=CARTESIAN_POINT('Ctrl Pts',(-0.211972685909792,7.19894710696887,
9.45510976419299E-17));
#14405=CARTESIAN_POINT('Ctrl Pts',(-0.22197690688827,7.21318605721376,1.07552855510562E-16));
#14406=CARTESIAN_POINT('Ctrl Pts',(-0.228265864693712,7.22213709472849,
1.15726156241153E-16));
#14407=CARTESIAN_POINT('Ctrl Pts',(-0.234059012930639,7.23142615662503,
5.59373896742589E-17));
#14408=CARTESIAN_POINT('Ctrl Pts',(-0.239308852044784,7.24101980913937,
5.20417042793042E-17));
#14409=CARTESIAN_POINT('Ctrl Pts',(-0.241553615206904,7.24512193061131,
5.03759596963439E-17));
#14410=CARTESIAN_POINT('Ctrl Pts',(-0.243698936078229,7.24927975670907,
3.19182285479356E-17));
#14411=CARTESIAN_POINT('Ctrl Pts',(-0.245740587550779,7.25349070851309,
3.46944695195361E-17));
#14412=CARTESIAN_POINT('Ctrl Pts',(-0.247686902746868,7.25750502711564,
3.73410720683434E-17));
#14413=CARTESIAN_POINT('Ctrl Pts',(-0.249535087968469,7.26155962917014,
8.85331702759656E-17));
#14414=CARTESIAN_POINT('Ctrl Pts',(-0.251281746281186,7.26565003442524,
8.84708972748172E-17));
#14415=CARTESIAN_POINT('Ctrl Pts',(-0.257537589409274,7.28030025732224,
8.82478598762239E-17));
#14416=CARTESIAN_POINT('Ctrl Pts',(-0.262498392567991,7.29541738447504,
6.01328869974533E-17));
#14417=CARTESIAN_POINT('Ctrl Pts',(-0.266024737720578,7.31089144318791,
6.93889390390723E-17));
#14418=CARTESIAN_POINT('Ctrl Pts',(-0.268541655860434,7.32193600558507,
7.60750141973437E-17));
#14419=CARTESIAN_POINT('Ctrl Pts',(-0.270326735192568,7.33316280454067,
8.51582814892351E-17));
#14420=CARTESIAN_POINT('Ctrl Pts',(-0.27139185115298,7.34450305084133,9.36750677027476E-17));
#14421=CARTESIAN_POINT('Ctrl Pts',(-0.271805172843737,7.34890367006852,
9.69800341180657E-17));
#14422=CARTESIAN_POINT('Ctrl Pts',(-0.272109971626923,7.35332134308501,
7.35479546497213E-17));
#14423=CARTESIAN_POINT('Ctrl Pts',(-0.272306550140188,7.35775189119246,
7.63278329429795E-17));
#14424=CARTESIAN_POINT('Ctrl Pts',(-0.272509050092771,7.36231589855408,
7.91914481633018E-17));
#14425=CARTESIAN_POINT('Ctrl Pts',(-0.27259625011216,7.3668837741178,8.11349244050912E-17));
#14426=CARTESIAN_POINT('Ctrl Pts',(-0.272569824655828,7.37144896955051,
8.32667268468867E-17));
#14427=CARTESIAN_POINT('Ctrl Pts',(-0.27247174711454,7.38839259912947,9.11788680556787E-17));
#14428=CARTESIAN_POINT('Ctrl Pts',(-0.270813092352919,7.40531022346617,
1.04217775009023E-16));
#14429=CARTESIAN_POINT('Ctrl Pts',(-0.267648460108694,7.42197081815956,
1.14491749414469E-16));
#14430=CARTESIAN_POINT('Ctrl Pts',(-0.265994317828667,7.43067925312638,
1.19861920144093E-16));
#14431=CARTESIAN_POINT('Ctrl Pts',(-0.263927817272562,7.43931723336003,
9.45136624417438E-17));
#14432=CARTESIAN_POINT('Ctrl Pts',(-0.261451366292174,7.44784875840811,
8.67361737988404E-17));
#14433=CARTESIAN_POINT('Ctrl Pts',(-0.260001054064173,7.45284517271178,
8.21813544338432E-17));
#14434=CARTESIAN_POINT('Ctrl Pts',(-0.25840948354909,7.45780668536454,3.82362151915691E-17));
#14435=CARTESIAN_POINT('Ctrl Pts',(-0.25667848349565,7.4627203082836,3.81639164714898E-17));
#14436=CARTESIAN_POINT('Ctrl Pts',(-0.251357933337885,7.47782324091796,
3.79416929274988E-17));
#14437=CARTESIAN_POINT('Ctrl Pts',(-0.244748714237808,7.49240631417947,
4.33000400033759E-17));
#14438=CARTESIAN_POINT('Ctrl Pts',(-0.23687440208594,7.50625495367809,4.16333634234434E-17));
#14439=CARTESIAN_POINT('Ctrl Pts',(-0.232807824863395,7.51340688782321,
4.07726318590114E-17));
#14440=CARTESIAN_POINT('Ctrl Pts',(-0.228399165702,7.52036724850155,8.09844648225997E-17));
#14441=CARTESIAN_POINT('Ctrl Pts',(-0.223669116907964,7.52707485423541,
6.24500451351651E-17));
#14442=CARTESIAN_POINT('Ctrl Pts',(-0.216422990525043,7.53735046892582,
3.40565225020369E-17));
#14443=CARTESIAN_POINT('Ctrl Pts',(-0.208418220052085,7.54704578415416,
-1.68665796639332E-17));
#14444=CARTESIAN_POINT('Ctrl Pts',(-0.199658669018713,7.55604261798761,
-1.38777878078145E-17));
#14445=CARTESIAN_POINT('Ctrl Pts',(-0.197072131758363,7.55869922057452,
-1.99860593395901E-17));
#14446=CARTESIAN_POINT('Ctrl Pts',(-0.194419691364069,7.56129478193143,
-1.04514705227716E-17));
#14447=CARTESIAN_POINT('Ctrl Pts',(-0.191704062602121,7.56382811505057,
-1.38777878078145E-17));
#14448=CARTESIAN_POINT('Origin',(-7.4,0.,-0.45));
#14449=CARTESIAN_POINT('Origin',(7.4,0.,-0.45));
#14450=CARTESIAN_POINT('Origin',(0.,7.4,-0.45));
#14451=CARTESIAN_POINT('Origin',(0.,-7.4,-0.45));
#14452=CARTESIAN_POINT('Origin',(-4.,0.,-2.7));
#14453=CARTESIAN_POINT('',(-4.35,4.28626379701574E-17,-2.4));
#14454=CARTESIAN_POINT('Origin',(-4.,0.,-2.4));
#14455=CARTESIAN_POINT('',(-4.35,4.28626379701574E-17,-3.));
#14456=CARTESIAN_POINT('',(-4.35,4.28626379701574E-17,-2.7));
#14457=CARTESIAN_POINT('Origin',(-4.,0.,-3.));
#14458=CARTESIAN_POINT('Origin',(4.,0.,-2.7));
#14459=CARTESIAN_POINT('',(3.65,4.28626379701574E-17,-2.4));
#14460=CARTESIAN_POINT('Origin',(4.,0.,-2.4));
#14461=CARTESIAN_POINT('',(3.65,4.28626379701574E-17,-3.));
#14462=CARTESIAN_POINT('',(3.65,4.28626379701574E-17,-2.7));
#14463=CARTESIAN_POINT('Origin',(4.,0.,-3.));
#14464=CARTESIAN_POINT('Origin',(0.,4.,-2.7));
#14465=CARTESIAN_POINT('',(-0.35,4.,-2.4));
#14466=CARTESIAN_POINT('Origin',(0.,4.,-2.4));
#14467=CARTESIAN_POINT('',(-0.35,4.,-3.));
#14468=CARTESIAN_POINT('',(-0.35,4.,-2.7));
#14469=CARTESIAN_POINT('Origin',(0.,4.,-3.));
#14470=CARTESIAN_POINT('Origin',(0.,-4.,-2.7));
#14471=CARTESIAN_POINT('',(-0.35,-4.,-2.4));
#14472=CARTESIAN_POINT('Origin',(0.,-4.,-2.4));
#14473=CARTESIAN_POINT('',(-0.35,-4.,-3.));
#14474=CARTESIAN_POINT('',(-0.35,-4.,-2.7));
#14475=CARTESIAN_POINT('Origin',(0.,-4.,-3.));
#14476=CARTESIAN_POINT('Origin',(0.,0.,-2.4));
#14477=CARTESIAN_POINT('',(-4.8,-5.8783046359073E-16,-2.4));
#14478=CARTESIAN_POINT('Origin',(0.,0.,-2.4));
#14479=CARTESIAN_POINT('',(-3.5,-4.28626379701574E-16,-2.4));
#14480=CARTESIAN_POINT('Origin',(0.,0.,-2.4));
#14481=CARTESIAN_POINT('Origin',(0.,0.,-3.));
#14482=CARTESIAN_POINT('',(-4.8,-5.8783046359073E-16,-3.));
#14483=CARTESIAN_POINT('',(-4.8,-5.8783046359073E-16,-3.));
#14484=CARTESIAN_POINT('Origin',(0.,0.,-3.));
#14485=CARTESIAN_POINT('Origin',(0.,0.,-3.));
#14486=CARTESIAN_POINT('',(-2.7,-3.30654635769785E-16,-3.));
#14487=CARTESIAN_POINT('Origin',(0.,0.,-3.));
#14488=CARTESIAN_POINT('Origin',(0.,0.,-2.4));
#14489=CARTESIAN_POINT('',(-3.5,-4.28626379701574E-16,-2.4));
#14490=CARTESIAN_POINT('Origin',(-1.29641016151378,-1.44544826719043,-0.8));
#14491=CARTESIAN_POINT('',(-1.68151315379565,-2.11246621596943,-0.8));
#14492=CARTESIAN_POINT('',(-1.68151315379565,-2.11246621596943,-0.8));
#14493=CARTESIAN_POINT('',(-1.37718656791819,-1.58535710713571,-0.8));
#14494=CARTESIAN_POINT('',(-1.37718656791819,-1.58535710713571,-0.8));
#14495=CARTESIAN_POINT('',(-1.29641016151378,-1.44544826719043,-0.8));
#14496=CARTESIAN_POINT('Origin',(-1.20358983848623,-2.88467875173176,-0.8));
#14497=CARTESIAN_POINT('',(-0.988692830768095,-2.51246621596944,-0.8));
#14498=CARTESIAN_POINT('',(-0.988692830768095,-2.51246621596944,-0.8));
#14499=CARTESIAN_POINT('',(-0.684366244890641,-1.98535710713571,-0.8));
#14500=CARTESIAN_POINT('',(-1.20358983848623,-2.88467875173176,-0.8));
#14501=CARTESIAN_POINT('',(-0.684366244890641,-1.98535710713571,-0.8));
#14502=CARTESIAN_POINT('Origin',(-0.603589838486224,1.84544826719043,-0.8));
#14503=CARTESIAN_POINT('',(-0.988692830768093,2.51246621596944,-0.8));
#14504=CARTESIAN_POINT('',(-0.988692830768093,2.51246621596944,-0.8));
#14505=CARTESIAN_POINT('',(-0.684366244890639,1.98535710713571,-0.8));
#14506=CARTESIAN_POINT('',(-0.684366244890639,1.98535710713571,-0.8));
#14507=CARTESIAN_POINT('',(-0.603589838486224,1.84544826719043,-0.8));
#14508=CARTESIAN_POINT('Origin',(-1.89641016151378,2.48467875173176,-0.8));
#14509=CARTESIAN_POINT('',(-1.68151315379564,2.11246621596944,-0.8));
#14510=CARTESIAN_POINT('',(-1.68151315379564,2.11246621596944,-0.8));
#14511=CARTESIAN_POINT('',(-1.37718656791819,1.58535710713571,-0.8));
#14512=CARTESIAN_POINT('',(-1.89641016151378,2.48467875173176,-0.8));
#14513=CARTESIAN_POINT('',(-1.37718656791819,1.58535710713571,-0.8));
#14514=CARTESIAN_POINT('Origin',(0.,0.,-0.8));
#14515=CARTESIAN_POINT('',(2.67020598456374,-0.4,-0.8));
#14516=CARTESIAN_POINT('',(2.67020598456374,-0.4,-0.8));
#14517=CARTESIAN_POINT('',(2.67020598456374,0.4,-0.8));
#14518=CARTESIAN_POINT('Origin',(0.,0.,-0.8));
#14519=CARTESIAN_POINT('',(2.67020598456374,0.4,-0.8));
#14520=CARTESIAN_POINT('Origin',(0.,0.,-0.8));
#14521=CARTESIAN_POINT('',(-2.7,-3.30654635769785E-16,-0.8));
#14522=CARTESIAN_POINT('Origin',(0.,0.,-0.8));
#14523=CARTESIAN_POINT('Origin',(0.,0.,-0.8));
#14524=CARTESIAN_POINT('',(2.06155281280883,-0.4,-0.8));
#14525=CARTESIAN_POINT('',(1.9,-0.4,-0.8));
#14526=CARTESIAN_POINT('Origin',(0.,0.,-0.8));
#14527=CARTESIAN_POINT('Origin',(0.,0.,-0.8));
#14528=CARTESIAN_POINT('',(2.06155281280883,0.4,-0.8));
#14529=CARTESIAN_POINT('Origin',(0.,0.,-0.8));
#14530=CARTESIAN_POINT('',(3.1,0.4,-0.8));
#14531=CARTESIAN_POINT('',(-1.7,-2.0818995585505E-16,-0.8));
#14532=CARTESIAN_POINT('Origin',(0.,0.,-0.8));
#14533=CARTESIAN_POINT('Origin',(0.,0.,-0.8));
#14534=CARTESIAN_POINT('',(2.06155281280883,0.4,-0.8));
#14535=CARTESIAN_POINT('Origin',(0.,0.,-0.8));
#14536=CARTESIAN_POINT('Origin',(0.,0.,-0.8));
#14537=CARTESIAN_POINT('',(-1.7,-2.0818995585505E-16,-0.8));
#14538=CARTESIAN_POINT('Origin',(0.,0.,-0.8));
#14539=CARTESIAN_POINT('',(2.06155281280883,-0.4,-0.8));
#14540=CARTESIAN_POINT('Origin',(3.1,0.4,-0.8));
#14541=CARTESIAN_POINT('Origin',(0.,0.,0.));
#14542=CARTESIAN_POINT('',(-8.2,-1.00421037530083E-15,0.));
#14543=CARTESIAN_POINT('Origin',(0.,0.,0.));
#14544=CARTESIAN_POINT('Origin',(1.9,-0.4,-0.8));
#14545=CARTESIAN_POINT('Origin',(0.,0.,-0.8));
#14546=CARTESIAN_POINT('',(-8.2,-1.00421037530083E-15,-0.8));
#14547=CARTESIAN_POINT('',(0.,0.,0.));
#14548=CARTESIAN_POINT('Ctrl Pts',(6.375,0.,-0.1));
#14549=CARTESIAN_POINT('Ctrl Pts',(6.375,6.375,-0.1));
#14550=CARTESIAN_POINT('Ctrl Pts',(0.,6.375,-0.1));
#14551=CARTESIAN_POINT('Ctrl Pts',(-6.375,6.375,-0.1));
#14552=CARTESIAN_POINT('Ctrl Pts',(-6.375,0.,-0.1));
#14553=CARTESIAN_POINT('Ctrl Pts',(-6.375,-6.375,-0.1));
#14554=CARTESIAN_POINT('Ctrl Pts',(0.,-6.375,-0.1));
#14555=CARTESIAN_POINT('Ctrl Pts',(6.375,-6.375,-0.1));
#14556=CARTESIAN_POINT('Ctrl Pts',(6.375,0.,-0.1));
#14557=CARTESIAN_POINT('Ctrl Pts',(6.375,0.,3.06161699786838E-18));
#14558=CARTESIAN_POINT('Ctrl Pts',(6.375,6.375,3.06161699786838E-18));
#14559=CARTESIAN_POINT('Ctrl Pts',(0.,6.375,0.));
#14560=CARTESIAN_POINT('Ctrl Pts',(-6.375,6.375,-3.06161699786838E-18));
#14561=CARTESIAN_POINT('Ctrl Pts',(-6.375,0.,-3.06161699786838E-18));
#14562=CARTESIAN_POINT('Ctrl Pts',(-6.375,-6.375,-3.06161699786838E-18));
#14563=CARTESIAN_POINT('Ctrl Pts',(0.,-6.375,0.));
#14564=CARTESIAN_POINT('Ctrl Pts',(6.375,-6.375,3.06161699786838E-18));
#14565=CARTESIAN_POINT('Ctrl Pts',(6.375,0.,3.06161699786838E-18));
#14566=CARTESIAN_POINT('Ctrl Pts',(6.6,0.,0.));
#14567=CARTESIAN_POINT('Ctrl Pts',(6.6,6.6,0.));
#14568=CARTESIAN_POINT('Ctrl Pts',(0.,6.6,0.));
#14569=CARTESIAN_POINT('Ctrl Pts',(-6.6,6.6,0.));
#14570=CARTESIAN_POINT('Ctrl Pts',(-6.6,0.,0.));
#14571=CARTESIAN_POINT('Ctrl Pts',(-6.6,-6.6,0.));
#14572=CARTESIAN_POINT('Ctrl Pts',(0.,-6.6,0.));
#14573=CARTESIAN_POINT('Ctrl Pts',(6.6,-6.6,0.));
#14574=CARTESIAN_POINT('Ctrl Pts',(6.6,0.,0.));
#14575=CARTESIAN_POINT('Ctrl Pts',(6.825,0.,-3.06161699786838E-18));
#14576=CARTESIAN_POINT('Ctrl Pts',(6.825,6.825,-3.06161699786838E-18));
#14577=CARTESIAN_POINT('Ctrl Pts',(0.,6.825,0.));
#14578=CARTESIAN_POINT('Ctrl Pts',(-6.825,6.825,3.06161699786838E-18));
#14579=CARTESIAN_POINT('Ctrl Pts',(-6.825,0.,3.06161699786838E-18));
#14580=CARTESIAN_POINT('Ctrl Pts',(-6.825,-6.825,3.06161699786838E-18));
#14581=CARTESIAN_POINT('Ctrl Pts',(0.,-6.825,0.));
#14582=CARTESIAN_POINT('Ctrl Pts',(6.825,-6.825,-3.06161699786838E-18));
#14583=CARTESIAN_POINT('Ctrl Pts',(6.825,0.,-3.06161699786838E-18));
#14584=CARTESIAN_POINT('Ctrl Pts',(6.825,0.,-0.1));
#14585=CARTESIAN_POINT('Ctrl Pts',(6.825,6.825,-0.1));
#14586=CARTESIAN_POINT('Ctrl Pts',(0.,6.825,-0.1));
#14587=CARTESIAN_POINT('Ctrl Pts',(-6.825,6.825,-0.1));
#14588=CARTESIAN_POINT('Ctrl Pts',(-6.825,0.,-0.1));
#14589=CARTESIAN_POINT('Ctrl Pts',(-6.825,-6.825,-0.1));
#14590=CARTESIAN_POINT('Ctrl Pts',(0.,-6.825,-0.1));
#14591=CARTESIAN_POINT('Ctrl Pts',(6.825,-6.825,-0.1));
#14592=CARTESIAN_POINT('Ctrl Pts',(6.825,0.,-0.1));
#14593=CARTESIAN_POINT('Ctrl Pts',(6.825,0.,-0.2));
#14594=CARTESIAN_POINT('Ctrl Pts',(6.825,6.825,-0.2));
#14595=CARTESIAN_POINT('Ctrl Pts',(0.,6.825,-0.2));
#14596=CARTESIAN_POINT('Ctrl Pts',(-6.825,6.825,-0.2));
#14597=CARTESIAN_POINT('Ctrl Pts',(-6.825,0.,-0.2));
#14598=CARTESIAN_POINT('Ctrl Pts',(-6.825,-6.825,-0.2));
#14599=CARTESIAN_POINT('Ctrl Pts',(0.,-6.825,-0.2));
#14600=CARTESIAN_POINT('Ctrl Pts',(6.825,-6.825,-0.2));
#14601=CARTESIAN_POINT('Ctrl Pts',(6.825,0.,-0.2));
#14602=CARTESIAN_POINT('Ctrl Pts',(6.6,0.,-0.2));
#14603=CARTESIAN_POINT('Ctrl Pts',(6.6,6.6,-0.2));
#14604=CARTESIAN_POINT('Ctrl Pts',(0.,6.6,-0.2));
#14605=CARTESIAN_POINT('Ctrl Pts',(-6.6,6.6,-0.2));
#14606=CARTESIAN_POINT('Ctrl Pts',(-6.6,0.,-0.2));
#14607=CARTESIAN_POINT('Ctrl Pts',(-6.6,-6.6,-0.2));
#14608=CARTESIAN_POINT('Ctrl Pts',(0.,-6.6,-0.2));
#14609=CARTESIAN_POINT('Ctrl Pts',(6.6,-6.6,-0.2));
#14610=CARTESIAN_POINT('Ctrl Pts',(6.6,0.,-0.2));
#14611=CARTESIAN_POINT('Ctrl Pts',(6.375,0.,-0.2));
#14612=CARTESIAN_POINT('Ctrl Pts',(6.375,6.375,-0.2));
#14613=CARTESIAN_POINT('Ctrl Pts',(0.,6.375,-0.2));
#14614=CARTESIAN_POINT('Ctrl Pts',(-6.375,6.375,-0.2));
#14615=CARTESIAN_POINT('Ctrl Pts',(-6.375,0.,-0.2));
#14616=CARTESIAN_POINT('Ctrl Pts',(-6.375,-6.375,-0.2));
#14617=CARTESIAN_POINT('Ctrl Pts',(0.,-6.375,-0.2));
#14618=CARTESIAN_POINT('Ctrl Pts',(6.375,-6.375,-0.2));
#14619=CARTESIAN_POINT('Ctrl Pts',(6.375,0.,-0.2));
#14620=CARTESIAN_POINT('Ctrl Pts',(6.375,0.,-0.1));
#14621=CARTESIAN_POINT('Ctrl Pts',(6.375,6.375,-0.1));
#14622=CARTESIAN_POINT('Ctrl Pts',(0.,6.375,-0.1));
#14623=CARTESIAN_POINT('Ctrl Pts',(-6.375,6.375,-0.1));
#14624=CARTESIAN_POINT('Ctrl Pts',(-6.375,0.,-0.1));
#14625=CARTESIAN_POINT('Ctrl Pts',(-6.375,-6.375,-0.1));
#14626=CARTESIAN_POINT('Ctrl Pts',(0.,-6.375,-0.1));
#14627=CARTESIAN_POINT('Ctrl Pts',(6.375,-6.375,-0.1));
#14628=CARTESIAN_POINT('Ctrl Pts',(6.375,0.,-0.1));
#14629=CARTESIAN_POINT('',(6.375,0.,-0.1));
#14630=CARTESIAN_POINT('Origin',(6.6,0.,-0.1));
#14631=CARTESIAN_POINT('Origin',(0.,0.,-0.1));
#14632=CARTESIAN_POINT('',(0.,0.,0.));
#14633=CARTESIAN_POINT('Origin',(7.56604255869606,7.56604255869606,10.4));
#14634=CARTESIAN_POINT('',(7.56604255869606,7.56604255869606,7.4));
#14635=CARTESIAN_POINT('Origin',(7.56604255869606,7.56604255869606,10.4));
#14636=CARTESIAN_POINT('',(7.56604255869606,7.56604255869606,12.45));
#14637=CARTESIAN_POINT('Origin',(7.56604255869606,7.56604255869606,12.8));
#14638=CARTESIAN_POINT('',(6.11647365726364,9.01561146012848,10.4));
#14639=CARTESIAN_POINT('Origin',(5.86898628384834,9.26309883354377,10.4));
#14640=CARTESIAN_POINT('',(7.56604255869606,7.56604255869606,7.65));
#14641=CARTESIAN_POINT('Origin',(7.56604255869606,7.56604255869606,8.));
#14642=CARTESIAN_POINT('',(7.56604255869606,7.56604255869606,9.4));
#14643=CARTESIAN_POINT('Origin',(7.56604255869606,7.56604255869606,10.4));
#14644=CARTESIAN_POINT('',(9.26309883354377,5.86898628384835,10.05));
#14645=CARTESIAN_POINT('Origin',(9.26309883354377,5.86898628384834,10.4));
#14646=CARTESIAN_POINT('Origin',(7.00035713374682,7.00035713374682,8.));
#14647=CARTESIAN_POINT('',(6.78822509939086,6.78822509939086,7.65));
#14648=CARTESIAN_POINT('',(7.00035713374682,7.00035713374682,7.65));
#14649=CARTESIAN_POINT('Origin',(6.78822509939086,6.78822509939086,8.));
#14650=CARTESIAN_POINT('Origin',(8.69741340859454,5.30330085889911,10.4));
#14651=CARTESIAN_POINT('',(8.48528137423857,5.09116882454314,10.05));
#14652=CARTESIAN_POINT('',(8.69741340859454,5.30330085889911,10.05));
#14653=CARTESIAN_POINT('Origin',(8.48528137423857,5.09116882454314,10.4));
#14654=CARTESIAN_POINT('Origin',(7.00035713374682,7.00035713374682,12.8));
#14655=CARTESIAN_POINT('',(6.78822509939086,6.78822509939086,12.45));
#14656=CARTESIAN_POINT('',(7.00035713374682,7.00035713374682,12.45));
#14657=CARTESIAN_POINT('Origin',(6.78822509939086,6.78822509939086,12.8));
#14658=CARTESIAN_POINT('Origin',(5.30330085889911,8.69741340859454,10.4));
#14659=CARTESIAN_POINT('',(5.33865619795843,8.23779400082328,10.4));
#14660=CARTESIAN_POINT('',(5.5507882323144,8.44992603517924,10.4));
#14661=CARTESIAN_POINT('Origin',(5.09116882454314,8.48528137423857,10.4));
#14662=CARTESIAN_POINT('Origin',(6.78822509939086,6.78822509939086,10.4));
#14663=CARTESIAN_POINT('',(6.78822509939086,6.78822509939086,7.4));
#14664=CARTESIAN_POINT('Origin',(6.78822509939086,6.78822509939086,10.4));
#14665=CARTESIAN_POINT('',(6.78822509939086,6.78822509939086,8.6));
#14666=CARTESIAN_POINT('Origin',(6.78822509939086,6.78822509939086,10.4));
#14667=CARTESIAN_POINT('Origin',(6.78822509939086,6.78822509939086,10.4));
#14668=CARTESIAN_POINT('',(6.78822509939086,6.78822509939086,7.4));
#14669=CARTESIAN_POINT('Origin',(4.10121933088198,4.10121933088197,10.4));
#14670=CARTESIAN_POINT('',(3.30121933088198,4.90121933088198,11.8));
#14671=CARTESIAN_POINT('',(4.90121933088198,3.30121933088197,11.8));
#14672=CARTESIAN_POINT('',(4.10121933088198,4.10121933088198,11.8));
#14673=CARTESIAN_POINT('Origin',(4.10121933088198,4.10121933088197,10.4));
#14674=CARTESIAN_POINT('',(4.10121933088198,4.10121933088197,9.4));
#14675=CARTESIAN_POINT('Origin',(4.10121933088198,4.10121933088197,10.4));
#14676=CARTESIAN_POINT('Origin',(4.10121933088198,4.10121933088197,10.4));
#14677=CARTESIAN_POINT('',(4.10121933088198,4.10121933088197,9.4));
#14678=CARTESIAN_POINT('Origin',(4.10121933088198,4.10121933088197,10.4));
#14679=CARTESIAN_POINT('',(5.79827560572969,5.79827560572969,8.6));
#14680=CARTESIAN_POINT('',(4.10121933088198,4.10121933088197,8.6));
#14681=CARTESIAN_POINT('',(4.38406204335659,6.92964645562816,10.4));
#14682=CARTESIAN_POINT('Ctrl Pts',(4.38406204335659,6.92964645562816,10.4));
#14683=CARTESIAN_POINT('Ctrl Pts',(4.38406204335659,6.92964645562816,10.2865909205213));
#14684=CARTESIAN_POINT('Ctrl Pts',(4.39351442674295,6.9236969445152,10.1694312898585));
#14685=CARTESIAN_POINT('Ctrl Pts',(4.43298837551974,6.89848986805715,9.93661580499002));
#14686=CARTESIAN_POINT('Ctrl Pts',(4.46299641756371,6.87923453928561,9.82095741594961));
#14687=CARTESIAN_POINT('Ctrl Pts',(4.54148608145332,6.82767229358142,9.59933149392755));
#14688=CARTESIAN_POINT('Ctrl Pts',(4.59001683917394,6.79531113210536,9.49318037852834));
#14689=CARTESIAN_POINT('Ctrl Pts',(4.70067362633218,6.71923919982036,9.29696790693528));
#14690=CARTESIAN_POINT('Ctrl Pts',(4.762788529836,6.6755040740321,9.20690971951041));
#14691=CARTESIAN_POINT('Ctrl Pts',(4.89320891867947,6.5805026125348,9.04751240050683));
#14692=CARTESIAN_POINT('Ctrl Pts',(4.96603345147513,6.52596993125439,8.97266585747222));
#14693=CARTESIAN_POINT('Ctrl Pts',(5.12191066634055,6.40435811856043,8.84062578857748));
#14694=CARTESIAN_POINT('Ctrl Pts',(5.20494441036095,6.33726453633079,8.78342321653815));
#14695=CARTESIAN_POINT('Ctrl Pts',(5.37489594368109,6.1937760462778,8.69145891577341));
#14696=CARTESIAN_POINT('Ctrl Pts',(5.46194275097718,6.1172507384193,8.65662409391343));
#14697=CARTESIAN_POINT('Ctrl Pts',(5.63354106814756,5.95959648341559,8.61088911405032));
#14698=CARTESIAN_POINT('Ctrl Pts',(5.71808984906397,5.87846136239541,8.6));
#14699=CARTESIAN_POINT('Ctrl Pts',(5.79827560572969,5.79827560572969,8.6));
#14700=CARTESIAN_POINT('Ctrl Pts',(5.79827560572969,5.79827560572969,8.6));
#14701=CARTESIAN_POINT('Ctrl Pts',(5.87846136239541,5.71808984906396,8.6));
#14702=CARTESIAN_POINT('Ctrl Pts',(5.95959648341559,5.63354106814755,8.61088911405032));
#14703=CARTESIAN_POINT('Ctrl Pts',(6.11725073841931,5.46194275097717,8.65662409391343));
#14704=CARTESIAN_POINT('Ctrl Pts',(6.1937760462778,5.37489594368109,8.69145891577341));
#14705=CARTESIAN_POINT('Ctrl Pts',(6.3372645363308,5.20494441036095,8.78342321653815));
#14706=CARTESIAN_POINT('Ctrl Pts',(6.40435811856043,5.12191066634055,8.84062578857748));
#14707=CARTESIAN_POINT('Ctrl Pts',(6.5259699312544,4.96603345147512,8.97266585747222));
#14708=CARTESIAN_POINT('Ctrl Pts',(6.5805026125348,4.89320891867947,9.04751240050683));
#14709=CARTESIAN_POINT('Ctrl Pts',(6.6755040740321,4.76278852983599,9.20690971951041));
#14710=CARTESIAN_POINT('Ctrl Pts',(6.71923919982036,4.70067362633218,9.29696790693528));
#14711=CARTESIAN_POINT('Ctrl Pts',(6.79531113210536,4.59001683917394,9.49318037852834));
#14712=CARTESIAN_POINT('Ctrl Pts',(6.82767229358142,4.54148608145332,9.59933149392755));
#14713=CARTESIAN_POINT('Ctrl Pts',(6.87923453928561,4.46299641756371,9.82095741594961));
#14714=CARTESIAN_POINT('Ctrl Pts',(6.89848986805715,4.43298837551974,9.93661580499002));
#14715=CARTESIAN_POINT('Ctrl Pts',(6.9236969445152,4.39351442674295,10.1694312898585));
#14716=CARTESIAN_POINT('Ctrl Pts',(6.92964645562817,4.38406204335659,10.2865909205213));
#14717=CARTESIAN_POINT('Ctrl Pts',(6.92964645562817,4.38406204335659,10.5134090794787));
#14718=CARTESIAN_POINT('Ctrl Pts',(6.9236969445152,4.39351442674295,10.6305687101415));
#14719=CARTESIAN_POINT('Ctrl Pts',(6.89848986805715,4.43298837551974,10.86338419501));
#14720=CARTESIAN_POINT('Ctrl Pts',(6.87923453928561,4.46299641756371,10.9790425840504));
#14721=CARTESIAN_POINT('Ctrl Pts',(6.82767229358142,4.54148608145332,11.2006685060725));
#14722=CARTESIAN_POINT('Ctrl Pts',(6.79531113210536,4.59001683917394,11.3068196214717));
#14723=CARTESIAN_POINT('Ctrl Pts',(6.71923919982036,4.70067362633218,11.5030320930647));
#14724=CARTESIAN_POINT('Ctrl Pts',(6.6755040740321,4.76278852983599,11.5930902804896));
#14725=CARTESIAN_POINT('Ctrl Pts',(6.5805026125348,4.89320891867947,11.7524875994932));
#14726=CARTESIAN_POINT('Ctrl Pts',(6.5259699312544,4.96603345147512,11.8273341425278));
#14727=CARTESIAN_POINT('Ctrl Pts',(6.40435811856043,5.12191066634055,11.9593742114225));
#14728=CARTESIAN_POINT('Ctrl Pts',(6.3372645363308,5.20494441036095,12.0165767834619));
#14729=CARTESIAN_POINT('Ctrl Pts',(6.1937760462778,5.37489594368109,12.1085410842266));
#14730=CARTESIAN_POINT('Ctrl Pts',(6.11725073841931,5.46194275097717,12.1433759060866));
#14731=CARTESIAN_POINT('Ctrl Pts',(5.95959648341559,5.63354106814755,12.1891108859497));
#14732=CARTESIAN_POINT('Ctrl Pts',(5.87846136239541,5.71808984906396,12.2));
#14733=CARTESIAN_POINT('Ctrl Pts',(5.71808984906397,5.87846136239541,12.2));
#14734=CARTESIAN_POINT('Ctrl Pts',(5.63354106814756,5.95959648341559,12.1891108859497));
#14735=CARTESIAN_POINT('Ctrl Pts',(5.46194275097718,6.1172507384193,12.1433759060866));
#14736=CARTESIAN_POINT('Ctrl Pts',(5.37489594368109,6.19377604627779,12.1085410842266));
#14737=CARTESIAN_POINT('Ctrl Pts',(5.20494441036096,6.33726453633079,12.0165767834619));
#14738=CARTESIAN_POINT('Ctrl Pts',(5.12191066634055,6.40435811856043,11.9593742114225));
#14739=CARTESIAN_POINT('Ctrl Pts',(4.96603345147513,6.52596993125439,11.8273341425278));
#14740=CARTESIAN_POINT('Ctrl Pts',(4.89320891867947,6.5805026125348,11.7524875994932));
#14741=CARTESIAN_POINT('Ctrl Pts',(4.762788529836,6.6755040740321,11.5930902804896));
#14742=CARTESIAN_POINT('Ctrl Pts',(4.70067362633218,6.71923919982036,11.5030320930647));
#14743=CARTESIAN_POINT('Ctrl Pts',(4.59001683917394,6.79531113210536,11.3068196214717));
#14744=CARTESIAN_POINT('Ctrl Pts',(4.54148608145332,6.82767229358142,11.2006685060725));
#14745=CARTESIAN_POINT('Ctrl Pts',(4.46299641756371,6.87923453928561,10.9790425840504));
#14746=CARTESIAN_POINT('Ctrl Pts',(4.43298837551974,6.89848986805715,10.86338419501));
#14747=CARTESIAN_POINT('Ctrl Pts',(4.39351442674295,6.9236969445152,10.6305687101415));
#14748=CARTESIAN_POINT('Ctrl Pts',(4.38406204335659,6.92964645562816,10.5134090794787));
#14749=CARTESIAN_POINT('Ctrl Pts',(4.38406204335659,6.92964645562816,10.4));
#14750=CARTESIAN_POINT('Origin',(4.10121933088198,4.10121933088197,10.4));
#14751=CARTESIAN_POINT('',(5.11045241245046,3.51045241245046,11.8));
#14752=CARTESIAN_POINT('',(4.90121933088198,3.30121933088197,11.8));
#14753=CARTESIAN_POINT('',(3.51045241245046,5.11045241245046,11.8));
#14754=CARTESIAN_POINT('',(3.30121933088198,4.90121933088198,11.8));
#14755=CARTESIAN_POINT('Ctrl Pts',(5.11045241245046,3.51045241245046,11.8));
#14756=CARTESIAN_POINT('Ctrl Pts',(5.1392884847325,3.46847338586213,11.7595342292169));
#14757=CARTESIAN_POINT('Ctrl Pts',(5.16604843385166,3.42840683238517,11.7168862526028));
#14758=CARTESIAN_POINT('Ctrl Pts',(5.23513875566729,3.32263882324339,11.5932427410358));
#14759=CARTESIAN_POINT('Ctrl Pts',(5.27571579225433,3.25752083254924,11.5033547023141));
#14760=CARTESIAN_POINT('Ctrl Pts',(5.34585685398518,3.14108796317008,11.3074382155668));
#14761=CARTESIAN_POINT('Ctrl Pts',(5.37545194601955,3.08978936367632,11.2014112168311));
#14762=CARTESIAN_POINT('Ctrl Pts',(5.42242408885916,3.00659260724669,10.9798841112198));
#14763=CARTESIAN_POINT('Ctrl Pts',(5.4398572338365,2.97464720753252,10.8641950362263));
#14764=CARTESIAN_POINT('Ctrl Pts',(5.4626589384034,2.93256373453205,10.6311198770982));
#14765=CARTESIAN_POINT('Ctrl Pts',(5.46802759881639,2.92244318654482,10.5137306388427));
#14766=CARTESIAN_POINT('Ctrl Pts',(5.46802759881639,2.92244318654482,10.2862693611573));
#14767=CARTESIAN_POINT('Ctrl Pts',(5.4626589384034,2.93256373453205,10.1688801229018));
#14768=CARTESIAN_POINT('Ctrl Pts',(5.4398572338365,2.97464720753252,9.93580496377367));
#14769=CARTESIAN_POINT('Ctrl Pts',(5.42242408885916,3.00659260724669,9.82011588878015));
#14770=CARTESIAN_POINT('Ctrl Pts',(5.37545194601955,3.08978936367632,9.59858878316889));
#14771=CARTESIAN_POINT('Ctrl Pts',(5.34585685398518,3.14108796317009,9.49256178443324));
#14772=CARTESIAN_POINT('Ctrl Pts',(5.27571579225433,3.25752083254924,9.29664529768588));
#14773=CARTESIAN_POINT('Ctrl Pts',(5.23513875566729,3.32263882324339,9.20675725896418));
#14774=CARTESIAN_POINT('Ctrl Pts',(5.14624797411185,3.45871867855604,9.0476789960669));
#14775=CARTESIAN_POINT('Ctrl Pts',(5.09486035652437,3.53443821623447,8.97294373554617));
#14776=CARTESIAN_POINT('Ctrl Pts',(4.979089803435,3.69574353629806,8.84100693089275));
#14777=CARTESIAN_POINT('Ctrl Pts',(4.91468655172761,3.78130694811503,8.78379586536565));
#14778=CARTESIAN_POINT('Ctrl Pts',(4.77558243884065,3.95553264505421,8.6917407501633));
#14779=CARTESIAN_POINT('Ctrl Pts',(4.70074823922057,4.04432816738502,8.65682358615613));
#14780=CARTESIAN_POINT('Ctrl Pts',(4.54519137669676,4.21839539199965,8.61094721784197));
#14781=CARTESIAN_POINT('Ctrl Pts',(4.46446085591589,4.3036632307973,8.6));
#14782=CARTESIAN_POINT('Ctrl Pts',(4.3036632307973,4.46446085591589,8.6));
#14783=CARTESIAN_POINT('Ctrl Pts',(4.21839539199965,4.54519137669676,8.61094721784197));
#14784=CARTESIAN_POINT('Ctrl Pts',(4.04432816738502,4.70074823922057,8.65682358615613));
#14785=CARTESIAN_POINT('Ctrl Pts',(3.95553264505421,4.77558243884065,8.6917407501633));
#14786=CARTESIAN_POINT('Ctrl Pts',(3.78130694811503,4.91468655172761,8.78379586536565));
#14787=CARTESIAN_POINT('Ctrl Pts',(3.69574353629807,4.979089803435,8.84100693089275));
#14788=CARTESIAN_POINT('Ctrl Pts',(3.53443821623447,5.09486035652437,8.97294373554617));
#14789=CARTESIAN_POINT('Ctrl Pts',(3.45871867855604,5.14624797411185,9.0476789960669));
#14790=CARTESIAN_POINT('Ctrl Pts',(3.3226388232434,5.23513875566729,9.20675725896418));
#14791=CARTESIAN_POINT('Ctrl Pts',(3.25752083254925,5.27571579225433,9.29664529768588));
#14792=CARTESIAN_POINT('Ctrl Pts',(3.14108796317009,5.34585685398517,9.49256178443324));
#14793=CARTESIAN_POINT('Ctrl Pts',(3.08978936367632,5.37545194601955,9.59858878316889));
#14794=CARTESIAN_POINT('Ctrl Pts',(3.0065926072467,5.42242408885916,9.82011588878015));
#14795=CARTESIAN_POINT('Ctrl Pts',(2.97464720753252,5.4398572338365,9.93580496377367));
#14796=CARTESIAN_POINT('Ctrl Pts',(2.93256373453205,5.4626589384034,10.1688801229018));
#14797=CARTESIAN_POINT('Ctrl Pts',(2.92244318654482,5.46802759881639,10.2862693611573));
#14798=CARTESIAN_POINT('Ctrl Pts',(2.92244318654482,5.46802759881639,10.4));
#14799=CARTESIAN_POINT('Ctrl Pts',(2.92244318654482,5.46802759881639,10.5137306388427));
#14800=CARTESIAN_POINT('Ctrl Pts',(2.93256373453206,5.4626589384034,10.6311198770982));
#14801=CARTESIAN_POINT('Ctrl Pts',(2.97464720753252,5.4398572338365,10.8641950362263));
#14802=CARTESIAN_POINT('Ctrl Pts',(3.0065926072467,5.42242408885916,10.9798841112198));
#14803=CARTESIAN_POINT('Ctrl Pts',(3.08978936367632,5.37545194601955,11.2014112168311));
#14804=CARTESIAN_POINT('Ctrl Pts',(3.14108796317009,5.34585685398518,11.3074382155668));
#14805=CARTESIAN_POINT('Ctrl Pts',(3.25752083254925,5.27571579225433,11.5033547023141));
#14806=CARTESIAN_POINT('Ctrl Pts',(3.3226388232434,5.23513875566729,11.5932427410358));
#14807=CARTESIAN_POINT('Ctrl Pts',(3.42840683238549,5.16604843385145,11.7168862526031));
#14808=CARTESIAN_POINT('Ctrl Pts',(3.46847338586204,5.13928848473256,11.7595342292168));
#14809=CARTESIAN_POINT('Ctrl Pts',(3.51045241245046,5.11045241245046,11.8));
#14810=CARTESIAN_POINT('Origin',(0.,0.,8.4));
#14811=CARTESIAN_POINT('',(-6.2,-7.59281015471359E-16,11.8));
#14812=CARTESIAN_POINT('Origin',(0.,0.,11.8));
#14813=CARTESIAN_POINT('',(-6.2,-7.59281015471359E-16,8.4));
#14814=CARTESIAN_POINT('',(-6.2,-7.59281015471359E-16,8.4));
#14815=CARTESIAN_POINT('Origin',(0.,0.,8.4));
#14816=CARTESIAN_POINT('Origin',(0.,0.,11.8));
#14817=CARTESIAN_POINT('Origin',(0.,0.,8.4));
#14818=CARTESIAN_POINT('',(-8.2,-1.00421037530083E-15,12.8));
#14819=CARTESIAN_POINT('Origin',(0.,0.,12.8));
#14820=CARTESIAN_POINT('',(-8.2,-1.00421037530083E-15,8.4));
#14821=CARTESIAN_POINT('',(-8.2,-1.00421037530083E-15,8.4));
#14822=CARTESIAN_POINT('Origin',(0.,0.,8.4));
#14823=CARTESIAN_POINT('Origin',(-7.4,0.,10.6));
#14824=CARTESIAN_POINT('',(-7.75,4.28626379701574E-17,12.8));
#14825=CARTESIAN_POINT('Origin',(-7.4,0.,12.8));
#14826=CARTESIAN_POINT('',(-7.75,4.28626379701574E-17,8.4));
#14827=CARTESIAN_POINT('',(-7.75,4.28626379701574E-17,10.6));
#14828=CARTESIAN_POINT('Origin',(-7.4,0.,8.4));
#14829=CARTESIAN_POINT('Origin',(7.4,0.,10.6));
#14830=CARTESIAN_POINT('',(7.05,4.28626379701574E-17,12.8));
#14831=CARTESIAN_POINT('Origin',(7.4,0.,12.8));
#14832=CARTESIAN_POINT('',(7.05,4.28626379701574E-17,8.4));
#14833=CARTESIAN_POINT('',(7.05,4.28626379701574E-17,10.6));
#14834=CARTESIAN_POINT('Origin',(7.4,0.,8.4));
#14835=CARTESIAN_POINT('Origin',(0.,7.4,10.6));
#14836=CARTESIAN_POINT('',(-0.35,7.4,12.8));
#14837=CARTESIAN_POINT('Origin',(0.,7.4,12.8));
#14838=CARTESIAN_POINT('',(-0.35,7.4,8.4));
#14839=CARTESIAN_POINT('',(-0.35,7.4,10.6));
#14840=CARTESIAN_POINT('Origin',(0.,7.4,8.4));
#14841=CARTESIAN_POINT('Origin',(0.,-7.4,10.6));
#14842=CARTESIAN_POINT('',(-0.35,-7.4,12.8));
#14843=CARTESIAN_POINT('Origin',(0.,-7.4,12.8));
#14844=CARTESIAN_POINT('',(-0.35,-7.4,8.4));
#14845=CARTESIAN_POINT('',(-0.35,-7.4,10.6));
#14846=CARTESIAN_POINT('Origin',(0.,-7.4,8.4));
#14847=CARTESIAN_POINT('Origin',(0.,0.,11.4));
#14848=CARTESIAN_POINT('',(-1.7,-2.0818995585505E-16,11.6));
#14849=CARTESIAN_POINT('Origin',(0.,0.,11.6));
#14850=CARTESIAN_POINT('',(-1.7,-2.0818995585505E-16,11.4));
#14851=CARTESIAN_POINT('',(-1.7,-2.0818995585505E-16,11.4));
#14852=CARTESIAN_POINT('Origin',(0.,0.,11.4));
#14853=CARTESIAN_POINT('Origin',(0.,0.,11.4));
#14854=CARTESIAN_POINT('',(-2.1,-2.57175827820944E-16,11.4));
#14855=CARTESIAN_POINT('Origin',(0.,0.,11.4));
#14856=CARTESIAN_POINT('Origin',(0.,0.,11.8));
#14857=CARTESIAN_POINT('',(-1.7,-2.0818995585505E-16,11.8));
#14858=CARTESIAN_POINT('Origin',(0.,0.,11.8));
#14859=CARTESIAN_POINT('',(-1.1,-1.34711147906209E-16,11.8));
#14860=CARTESIAN_POINT('Origin',(0.,0.,11.8));
#14861=CARTESIAN_POINT('Origin',(0.,0.,11.6));
#14862=CARTESIAN_POINT('',(-1.1,-1.34711147906209E-16,11.6));
#14863=CARTESIAN_POINT('',(-1.1,-1.34711147906209E-16,11.6));
#14864=CARTESIAN_POINT('Origin',(0.,0.,11.6));
#14865=CARTESIAN_POINT('Origin',(0.,0.,11.6));
#14866=CARTESIAN_POINT('',(-2.1,-2.57175827820944E-16,11.8));
#14867=CARTESIAN_POINT('Origin',(0.,0.,11.8));
#14868=CARTESIAN_POINT('',(-2.1,-2.57175827820944E-16,11.6));
#14869=CARTESIAN_POINT('Origin',(0.,0.,11.6));
#14870=CARTESIAN_POINT('Origin',(0.,0.,11.8));
#14871=CARTESIAN_POINT('Origin',(0.,0.,11.8));
#14872=CARTESIAN_POINT('',(-1.7,-2.0818995585505E-16,12.8));
#14873=CARTESIAN_POINT('Origin',(0.,0.,12.8));
#14874=CARTESIAN_POINT('',(-1.7,-2.0818995585505E-16,11.8));
#14875=CARTESIAN_POINT('Origin',(0.,0.,12.8));
#14876=CARTESIAN_POINT('Origin',(0.,0.,8.4));
#14877=CARTESIAN_POINT('',(0.,0.,0.));
#14878=CARTESIAN_POINT('Origin',(0.7,0.,15.3));
#14879=CARTESIAN_POINT('',(0.7,0.,15.6));
#14880=CARTESIAN_POINT('',(1.,0.,15.6));
#14881=CARTESIAN_POINT('',(0.7,0.,15.6));
#14882=CARTESIAN_POINT('',(0.7,0.3,15.3));
#14883=CARTESIAN_POINT('Origin',(0.7,0.,15.3));
#14884=CARTESIAN_POINT('',(0.953939201416946,0.3,15.3));
#14885=CARTESIAN_POINT('',(0.7,0.3,15.3));
#14886=CARTESIAN_POINT('Ctrl Pts',(1.,-3.88578058618805E-16,15.6));
#14887=CARTESIAN_POINT('Ctrl Pts',(1.,0.0379164265292001,15.6));
#14888=CARTESIAN_POINT('Ctrl Pts',(0.997630133387832,0.0782037717481895,
15.5923748246511));
#14889=CARTESIAN_POINT('Ctrl Pts',(0.989071194990079,0.152052241900625,
15.5616848907033));
#14890=CARTESIAN_POINT('Ctrl Pts',(0.982993562614982,0.185631434471708,
15.5386326342402));
#14891=CARTESIAN_POINT('Ctrl Pts',(0.971486751729016,0.238640531261463,
15.4856235374505));
#14892=CARTESIAN_POINT('Ctrl Pts',(0.965284956103207,0.261686672615768,
15.4520475537716));
#14893=CARTESIAN_POINT('Ctrl Pts',(0.956437939057487,0.292372091609923,
15.3782107485428));
#14894=CARTESIAN_POINT('Ctrl Pts',(0.953939201416946,0.3,15.3379277253989));
#14895=CARTESIAN_POINT('Ctrl Pts',(0.953939201416946,0.3,15.3));
#14896=CARTESIAN_POINT('Origin',(0.7,0.,15.3));
#14897=CARTESIAN_POINT('',(0.953939201416946,-0.3,15.3));
#14898=CARTESIAN_POINT('Ctrl Pts',(0.953939201416946,-0.3,15.3));
#14899=CARTESIAN_POINT('Ctrl Pts',(0.953939201416946,-0.3,15.3379277253989));
#14900=CARTESIAN_POINT('Ctrl Pts',(0.956437939057487,-0.292372091609923,
15.3782107485428));
#14901=CARTESIAN_POINT('Ctrl Pts',(0.965284956103207,-0.261686672615768,
15.4520475537716));
#14902=CARTESIAN_POINT('Ctrl Pts',(0.971486751729016,-0.238640531261463,
15.4856235374505));
#14903=CARTESIAN_POINT('Ctrl Pts',(0.982993562614982,-0.185631434471709,
15.5386326342402));
#14904=CARTESIAN_POINT('Ctrl Pts',(0.989071194990079,-0.152052241900624,
15.5616848907033));
#14905=CARTESIAN_POINT('Ctrl Pts',(0.997630133387832,-0.0782037717481885,
15.5923748246511));
#14906=CARTESIAN_POINT('Ctrl Pts',(1.,-0.0379164265292007,15.6));
#14907=CARTESIAN_POINT('Ctrl Pts',(1.,-2.70616862252382E-16,15.6));
#14908=CARTESIAN_POINT('',(0.7,-0.3,15.3));
#14909=CARTESIAN_POINT('',(0.7,-0.3,15.3));
#14910=CARTESIAN_POINT('Origin',(0.7,0.,15.3));
#14911=CARTESIAN_POINT('',(0.7,0.,15.6));
#14912=CARTESIAN_POINT('Origin',(0.7,0.3,13.7));
#14913=CARTESIAN_POINT('',(0.953939201416946,0.3,13.7));
#14914=CARTESIAN_POINT('',(0.953939201416946,0.3,-0.800000000000001));
#14915=CARTESIAN_POINT('',(0.7,0.3,13.7));
#14916=CARTESIAN_POINT('',(0.7,0.3,15.3));
#14917=CARTESIAN_POINT('',(0.7,0.3,13.7));
#14918=CARTESIAN_POINT('Origin',(0.7,0.,13.7));
#14919=CARTESIAN_POINT('',(0.953939201416946,-0.3,13.7));
#14920=CARTESIAN_POINT('Ctrl Pts',(0.953939201416946,0.3,13.7));
#14921=CARTESIAN_POINT('Ctrl Pts',(0.953939201416946,0.3,13.6620722746011));
#14922=CARTESIAN_POINT('Ctrl Pts',(0.956437939057488,0.292372091609922,
13.6217892514572));
#14923=CARTESIAN_POINT('Ctrl Pts',(0.965284956103208,0.261686672615766,
13.5479524462284));
#14924=CARTESIAN_POINT('Ctrl Pts',(0.971486751729016,0.238640531261462,
13.5143764625495));
#14925=CARTESIAN_POINT('Ctrl Pts',(0.982993562614982,0.185631434471708,
13.4613673657598));
#14926=CARTESIAN_POINT('Ctrl Pts',(0.98907119499008,0.152052241900622,13.4383151092967));
#14927=CARTESIAN_POINT('Ctrl Pts',(0.997630133387832,0.078203771748188,
13.4076251753489));
#14928=CARTESIAN_POINT('Ctrl Pts',(1.,0.0379164265292003,13.4));
#14929=CARTESIAN_POINT('Ctrl Pts',(1.,-0.0379164265292001,13.4));
#14930=CARTESIAN_POINT('Ctrl Pts',(0.997630133387832,-0.0782037717481879,
13.4076251753489));
#14931=CARTESIAN_POINT('Ctrl Pts',(0.98907119499008,-0.152052241900622,
13.4383151092967));
#14932=CARTESIAN_POINT('Ctrl Pts',(0.982993562614982,-0.185631434471708,
13.4613673657598));
#14933=CARTESIAN_POINT('Ctrl Pts',(0.971486751729016,-0.238640531261463,
13.5143764625495));
#14934=CARTESIAN_POINT('Ctrl Pts',(0.965284956103208,-0.261686672615766,
13.5479524462284));
#14935=CARTESIAN_POINT('Ctrl Pts',(0.956437939057488,-0.292372091609922,
13.6217892514572));
#14936=CARTESIAN_POINT('Ctrl Pts',(0.953939201416946,-0.3,13.6620722746011));
#14937=CARTESIAN_POINT('Ctrl Pts',(0.953939201416946,-0.3,13.7));
#14938=CARTESIAN_POINT('',(0.7,-0.3,13.7));
#14939=CARTESIAN_POINT('Origin',(0.7,0.,13.7));
#14940=CARTESIAN_POINT('',(0.7,-0.3,13.7));
#14941=CARTESIAN_POINT('Origin',(0.7,-0.3,15.3));
#14942=CARTESIAN_POINT('',(0.953939201416946,-0.3,-0.800000000000001));
#14943=CARTESIAN_POINT('',(0.7,-0.3,13.7));
#14944=CARTESIAN_POINT('Origin',(0.7,0.,14.5));
#14945=CARTESIAN_POINT('Origin',(0.,0.,-0.8));
#14946=CARTESIAN_POINT('',(-1.,-1.22464679914735E-16,15.6));
#14947=CARTESIAN_POINT('Origin',(0.,0.,15.6));
#14948=CARTESIAN_POINT('Origin',(0.,0.,15.6));
#14949=CARTESIAN_POINT('',(-1.,-1.22464679914735E-16,13.1));
#14950=CARTESIAN_POINT('',(-1.,-1.22464679914735E-16,-0.8));
#14951=CARTESIAN_POINT('Origin',(0.,0.,13.1));
#14952=CARTESIAN_POINT('Origin',(0.7,-0.3,6.9));
#14953=CARTESIAN_POINT('',(0.953939201416946,-0.3,6.3));
#14954=CARTESIAN_POINT('',(0.953939201416946,-0.3,6.9));
#14955=CARTESIAN_POINT('',(0.953939201416946,-0.3,-0.8));
#14956=CARTESIAN_POINT('',(0.7,-0.3,6.3));
#14957=CARTESIAN_POINT('',(0.7,-0.3,6.3));
#14958=CARTESIAN_POINT('',(0.7,-0.3,6.9));
#14959=CARTESIAN_POINT('',(0.7,-0.3,6.3));
#14960=CARTESIAN_POINT('',(0.7,-0.3,6.9));
#14961=CARTESIAN_POINT('Origin',(0.7,2.77555756156289E-17,6.9));
#14962=CARTESIAN_POINT('',(0.953939201416946,0.3,6.9));
#14963=CARTESIAN_POINT('Ctrl Pts',(0.953939201416946,-0.3,6.9));
#14964=CARTESIAN_POINT('Ctrl Pts',(0.953939201416946,-0.3,6.93792772539893));
#14965=CARTESIAN_POINT('Ctrl Pts',(0.956437939057488,-0.292372091609921,
6.97821074854282));
#14966=CARTESIAN_POINT('Ctrl Pts',(0.965284956103208,-0.261686672615765,
7.05204755377161));
#14967=CARTESIAN_POINT('Ctrl Pts',(0.971486751729016,-0.238640531261463,
7.08562353745047));
#14968=CARTESIAN_POINT('Ctrl Pts',(0.982993562614982,-0.185631434471708,
7.13863263424022));
#14969=CARTESIAN_POINT('Ctrl Pts',(0.98907119499008,-0.152052241900622,
7.1616848907033));
#14970=CARTESIAN_POINT('Ctrl Pts',(0.997630133387832,-0.078203771748188,
7.19237482465107));
#14971=CARTESIAN_POINT('Ctrl Pts',(1.,-0.0379164265292003,7.2));
#14972=CARTESIAN_POINT('Ctrl Pts',(1.,0.0379164265292002,7.2));
#14973=CARTESIAN_POINT('Ctrl Pts',(0.997630133387832,0.0782037717481879,
7.19237482465107));
#14974=CARTESIAN_POINT('Ctrl Pts',(0.98907119499008,0.152052241900622,7.1616848907033));
#14975=CARTESIAN_POINT('Ctrl Pts',(0.982993562614982,0.185631434471708,
7.13863263424022));
#14976=CARTESIAN_POINT('Ctrl Pts',(0.971486751729016,0.238640531261462,
7.08562353745047));
#14977=CARTESIAN_POINT('Ctrl Pts',(0.965284956103208,0.261686672615765,
7.05204755377162));
#14978=CARTESIAN_POINT('Ctrl Pts',(0.956437939057488,0.292372091609922,
6.97821074854282));
#14979=CARTESIAN_POINT('Ctrl Pts',(0.953939201416946,0.3,6.93792772539893));
#14980=CARTESIAN_POINT('Ctrl Pts',(0.953939201416946,0.3,6.9));
#14981=CARTESIAN_POINT('',(0.7,0.3,6.9));
#14982=CARTESIAN_POINT('Origin',(0.7,2.77555756156289E-17,6.9));
#14983=CARTESIAN_POINT('',(0.7,0.3,6.9));
#14984=CARTESIAN_POINT('Origin',(0.7,0.3,6.3));
#14985=CARTESIAN_POINT('',(0.953939201416946,0.3,6.3));
#14986=CARTESIAN_POINT('',(0.953939201416946,0.3,-0.8));
#14987=CARTESIAN_POINT('',(0.7,0.3,6.3));
#14988=CARTESIAN_POINT('',(0.7,0.3,6.9));
#14989=CARTESIAN_POINT('',(0.7,0.3,6.3));
#14990=CARTESIAN_POINT('Origin',(0.7,-2.77555756156289E-17,6.3));
#14991=CARTESIAN_POINT('Ctrl Pts',(0.953939201416946,0.3,6.3));
#14992=CARTESIAN_POINT('Ctrl Pts',(0.953939201416946,0.3,6.26207227460108));
#14993=CARTESIAN_POINT('Ctrl Pts',(0.956437939057488,0.292372091609921,
6.22178925145718));
#14994=CARTESIAN_POINT('Ctrl Pts',(0.965284956103208,0.261686672615765,
6.14795244622839));
#14995=CARTESIAN_POINT('Ctrl Pts',(0.971486751729016,0.238640531261462,
6.11437646254953));
#14996=CARTESIAN_POINT('Ctrl Pts',(0.982993562614982,0.185631434471708,
6.06136736575978));
#14997=CARTESIAN_POINT('Ctrl Pts',(0.98907119499008,0.152052241900622,6.0383151092967));
#14998=CARTESIAN_POINT('Ctrl Pts',(0.997630133387832,0.078203771748188,
6.00762517534893));
#14999=CARTESIAN_POINT('Ctrl Pts',(1.,0.0379164265292002,6.));
#15000=CARTESIAN_POINT('Ctrl Pts',(1.,-0.0379164265292002,6.));
#15001=CARTESIAN_POINT('Ctrl Pts',(0.997630133387832,-0.0782037717481879,
6.00762517534893));
#15002=CARTESIAN_POINT('Ctrl Pts',(0.98907119499008,-0.152052241900622,
6.0383151092967));
#15003=CARTESIAN_POINT('Ctrl Pts',(0.982993562614982,-0.185631434471708,
6.06136736575978));
#15004=CARTESIAN_POINT('Ctrl Pts',(0.971486751729016,-0.238640531261463,
6.11437646254953));
#15005=CARTESIAN_POINT('Ctrl Pts',(0.965284956103208,-0.261686672615765,
6.14795244622839));
#15006=CARTESIAN_POINT('Ctrl Pts',(0.956437939057488,-0.292372091609922,
6.22178925145718));
#15007=CARTESIAN_POINT('Ctrl Pts',(0.953939201416946,-0.3,6.26207227460108));
#15008=CARTESIAN_POINT('Ctrl Pts',(0.953939201416946,-0.3,6.3));
#15009=CARTESIAN_POINT('Origin',(0.7,-2.77555756156289E-17,6.3));
#15010=CARTESIAN_POINT('Origin',(0.7,0.,6.6));
#15011=CARTESIAN_POINT('Origin',(0.7,-0.3,2.7));
#15012=CARTESIAN_POINT('',(0.953939201416946,-0.3,2.1));
#15013=CARTESIAN_POINT('',(0.953939201416946,-0.3,2.7));
#15014=CARTESIAN_POINT('',(0.953939201416946,-0.3,-0.8));
#15015=CARTESIAN_POINT('',(0.7,-0.3,2.1));
#15016=CARTESIAN_POINT('',(0.7,-0.3,2.1));
#15017=CARTESIAN_POINT('',(0.7,-0.3,2.7));
#15018=CARTESIAN_POINT('',(0.7,-0.3,2.1));
#15019=CARTESIAN_POINT('',(0.7,-0.3,2.7));
#15020=CARTESIAN_POINT('Origin',(0.7,2.77555756156289E-17,2.7));
#15021=CARTESIAN_POINT('',(0.953939201416946,0.3,2.7));
#15022=CARTESIAN_POINT('Ctrl Pts',(0.953939201416946,-0.3,2.7));
#15023=CARTESIAN_POINT('Ctrl Pts',(0.953939201416946,-0.3,2.73792772539892));
#15024=CARTESIAN_POINT('Ctrl Pts',(0.956437939057488,-0.292372091609922,
2.77821074854282));
#15025=CARTESIAN_POINT('Ctrl Pts',(0.965284956103208,-0.261686672615765,
2.85204755377162));
#15026=CARTESIAN_POINT('Ctrl Pts',(0.971486751729016,-0.238640531261463,
2.88562353745047));
#15027=CARTESIAN_POINT('Ctrl Pts',(0.982993562614982,-0.185631434471708,
2.93863263424022));
#15028=CARTESIAN_POINT('Ctrl Pts',(0.98907119499008,-0.152052241900623,
2.9616848907033));
#15029=CARTESIAN_POINT('Ctrl Pts',(0.997630133387832,-0.078203771748188,
2.99237482465107));
#15030=CARTESIAN_POINT('Ctrl Pts',(1.,-0.0379164265292003,3.));
#15031=CARTESIAN_POINT('Ctrl Pts',(1.,0.0379164265292002,3.));
#15032=CARTESIAN_POINT('Ctrl Pts',(0.997630133387832,0.0782037717481883,
2.99237482465107));
#15033=CARTESIAN_POINT('Ctrl Pts',(0.98907119499008,0.152052241900623,2.9616848907033));
#15034=CARTESIAN_POINT('Ctrl Pts',(0.982993562614982,0.185631434471708,
2.93863263424022));
#15035=CARTESIAN_POINT('Ctrl Pts',(0.971486751729016,0.238640531261463,
2.88562353745047));
#15036=CARTESIAN_POINT('Ctrl Pts',(0.965284956103208,0.261686672615765,
2.85204755377162));
#15037=CARTESIAN_POINT('Ctrl Pts',(0.956437939057488,0.292372091609922,
2.77821074854282));
#15038=CARTESIAN_POINT('Ctrl Pts',(0.953939201416946,0.3,2.73792772539893));
#15039=CARTESIAN_POINT('Ctrl Pts',(0.953939201416946,0.3,2.7));
#15040=CARTESIAN_POINT('',(0.7,0.3,2.7));
#15041=CARTESIAN_POINT('Origin',(0.7,2.77555756156289E-17,2.7));
#15042=CARTESIAN_POINT('',(0.7,0.3,2.7));
#15043=CARTESIAN_POINT('Origin',(0.7,0.3,2.1));
#15044=CARTESIAN_POINT('',(0.953939201416946,0.3,2.1));
#15045=CARTESIAN_POINT('',(0.953939201416946,0.3,-0.8));
#15046=CARTESIAN_POINT('',(0.7,0.3,2.1));
#15047=CARTESIAN_POINT('',(0.7,0.3,2.7));
#15048=CARTESIAN_POINT('',(0.7,0.3,2.1));
#15049=CARTESIAN_POINT('Origin',(0.7,0.,2.1));
#15050=CARTESIAN_POINT('Ctrl Pts',(0.953939201416946,0.3,2.1));
#15051=CARTESIAN_POINT('Ctrl Pts',(0.953939201416946,0.3,2.06207227460107));
#15052=CARTESIAN_POINT('Ctrl Pts',(0.956437939057488,0.292372091609922,
2.02178925145718));
#15053=CARTESIAN_POINT('Ctrl Pts',(0.965284956103208,0.261686672615766,
1.94795244622839));
#15054=CARTESIAN_POINT('Ctrl Pts',(0.971486751729016,0.238640531261463,
1.91437646254953));
#15055=CARTESIAN_POINT('Ctrl Pts',(0.982993562614982,0.185631434471708,
1.86136736575978));
#15056=CARTESIAN_POINT('Ctrl Pts',(0.98907119499008,0.152052241900622,1.8383151092967));
#15057=CARTESIAN_POINT('Ctrl Pts',(0.997630133387832,0.0782037717481874,
1.80762517534893));
#15058=CARTESIAN_POINT('Ctrl Pts',(1.,0.0379164265292002,1.8));
#15059=CARTESIAN_POINT('Ctrl Pts',(1.,-0.0379164265292002,1.8));
#15060=CARTESIAN_POINT('Ctrl Pts',(0.997630133387832,-0.0782037717481877,
1.80762517534893));
#15061=CARTESIAN_POINT('Ctrl Pts',(0.98907119499008,-0.152052241900622,
1.8383151092967));
#15062=CARTESIAN_POINT('Ctrl Pts',(0.982993562614982,-0.185631434471708,
1.86136736575978));
#15063=CARTESIAN_POINT('Ctrl Pts',(0.971486751729016,-0.238640531261463,
1.91437646254953));
#15064=CARTESIAN_POINT('Ctrl Pts',(0.965284956103208,-0.261686672615765,
1.94795244622839));
#15065=CARTESIAN_POINT('Ctrl Pts',(0.956437939057488,-0.292372091609922,
2.02178925145718));
#15066=CARTESIAN_POINT('Ctrl Pts',(0.953939201416946,-0.3,2.06207227460107));
#15067=CARTESIAN_POINT('Ctrl Pts',(0.953939201416946,-0.3,2.1));
#15068=CARTESIAN_POINT('Origin',(0.7,0.,2.1));
#15069=CARTESIAN_POINT('Origin',(0.7,0.,2.4));
#15070=CARTESIAN_POINT('Origin',(0.,0.,13.05));
#15071=CARTESIAN_POINT('',(-0.9,-1.10218211923262E-16,13.));
#15072=CARTESIAN_POINT('Origin',(0.,0.,13.));
#15073=CARTESIAN_POINT('',(-0.9,-1.10218211923262E-16,13.1));
#15074=CARTESIAN_POINT('',(-0.9,-1.10218211923262E-16,13.05));
#15075=CARTESIAN_POINT('Origin',(0.,0.,13.1));
#15076=CARTESIAN_POINT('Origin',(1.3,0.,13.));
#15077=CARTESIAN_POINT('',(-1.,1.22464679914735E-16,13.));
#15078=CARTESIAN_POINT('Origin',(0.,0.,13.));
#15079=CARTESIAN_POINT('Origin',(0.9,0.,13.1));
#15080=CARTESIAN_POINT('Origin',(0.,0.,0.4));
#15081=CARTESIAN_POINT('',(-1.4,-1.71450551880629E-16,0.4));
#15082=CARTESIAN_POINT('Origin',(0.,0.,0.4));
#15083=CARTESIAN_POINT('',(-1.,-1.22464679914735E-16,0.4));
#15084=CARTESIAN_POINT('Origin',(0.,0.,0.4));
#15085=CARTESIAN_POINT('Origin',(0.,0.,0.));
#15086=CARTESIAN_POINT('',(-1.4,-1.71450551880629E-16,0.));
#15087=CARTESIAN_POINT('Origin',(0.,0.,0.));
#15088=CARTESIAN_POINT('',(-1.,1.22464679914735E-16,0.));
#15089=CARTESIAN_POINT('Origin',(0.,0.,0.));
#15090=CARTESIAN_POINT('Origin',(0.,0.,0.));
#15091=CARTESIAN_POINT('',(-1.4,-1.71450551880629E-16,0.));
#15092=CARTESIAN_POINT('Origin',(0.,0.,-0.8));
#15093=CARTESIAN_POINT('',(-1.,-1.22464679914735E-16,-0.8));
#15094=CARTESIAN_POINT('',(-1.,-1.22464679914735E-16,-0.8));
#15095=CARTESIAN_POINT('Origin',(0.,0.,-0.8));
#15096=CARTESIAN_POINT('Origin',(0.,0.,-0.8));
#15097=CARTESIAN_POINT('',(-1.,-1.22464679914735E-16,-0.8));
#15098=CARTESIAN_POINT('Origin',(0.,0.,15.6));
#15099=CARTESIAN_POINT('Origin',(0.,0.,-0.8));
#15100=CARTESIAN_POINT('',(0.,0.,0.));
#15101=CARTESIAN_POINT('Origin',(0.,0.,0.4));
#15102=CARTESIAN_POINT('',(-1.,-1.22464679914735E-16,1.8));
#15103=CARTESIAN_POINT('Origin',(0.,0.,1.8));
#15104=CARTESIAN_POINT('',(-1.,-1.22464679914735E-16,0.4));
#15105=CARTESIAN_POINT('',(-1.,-1.22464679914735E-16,0.4));
#15106=CARTESIAN_POINT('Origin',(0.,0.,0.4));
#15107=CARTESIAN_POINT('Origin',(0.,0.,0.4));
#15108=CARTESIAN_POINT('',(-1.5,-1.83697019872103E-16,1.8));
#15109=CARTESIAN_POINT('Origin',(0.,0.,1.8));
#15110=CARTESIAN_POINT('',(-1.5,-1.83697019872103E-16,0.4));
#15111=CARTESIAN_POINT('',(-1.5,-1.83697019872103E-16,0.4));
#15112=CARTESIAN_POINT('Origin',(0.,0.,0.4));
#15113=CARTESIAN_POINT('Origin',(0.,0.,1.8));
#15114=CARTESIAN_POINT('Origin',(0.,0.,0.4));
#15115=CARTESIAN_POINT('',(0.,0.,0.));
#15116=CARTESIAN_POINT('Origin',(0.,0.,3.2));
#15117=CARTESIAN_POINT('',(-1.,-1.22464679914735E-16,6.));
#15118=CARTESIAN_POINT('Origin',(0.,0.,6.));
#15119=CARTESIAN_POINT('',(-1.,-1.22464679914735E-16,3.2));
#15120=CARTESIAN_POINT('',(-1.,-1.22464679914735E-16,3.2));
#15121=CARTESIAN_POINT('Origin',(0.,0.,3.2));
#15122=CARTESIAN_POINT('Origin',(0.,0.,3.2));
#15123=CARTESIAN_POINT('',(-1.5,-1.83697019872103E-16,6.));
#15124=CARTESIAN_POINT('Origin',(0.,0.,6.));
#15125=CARTESIAN_POINT('',(-1.5,-1.83697019872103E-16,3.2));
#15126=CARTESIAN_POINT('',(-1.5,-1.83697019872103E-16,3.2));
#15127=CARTESIAN_POINT('Origin',(0.,0.,3.2));
#15128=CARTESIAN_POINT('Origin',(0.,0.,6.));
#15129=CARTESIAN_POINT('Origin',(0.,0.,3.2));
#15130=CARTESIAN_POINT('',(0.,0.,0.));
#15131=CARTESIAN_POINT('Origin',(0.,0.,7.4));
#15132=CARTESIAN_POINT('',(-1.,-1.22464679914735E-16,11.2));
#15133=CARTESIAN_POINT('Origin',(0.,0.,11.2));
#15134=CARTESIAN_POINT('',(-1.,-1.22464679914735E-16,7.4));
#15135=CARTESIAN_POINT('',(-1.,-1.22464679914735E-16,7.4));
#15136=CARTESIAN_POINT('Origin',(0.,0.,7.4));
#15137=CARTESIAN_POINT('Origin',(0.,0.,7.4));
#15138=CARTESIAN_POINT('',(-1.5,-1.83697019872103E-16,11.2));
#15139=CARTESIAN_POINT('Origin',(0.,0.,11.2));
#15140=CARTESIAN_POINT('',(-1.5,-1.83697019872103E-16,7.4));
#15141=CARTESIAN_POINT('',(-1.5,-1.83697019872103E-16,7.4));
#15142=CARTESIAN_POINT('Origin',(0.,0.,7.4));
#15143=CARTESIAN_POINT('Origin',(0.,0.,11.2));
#15144=CARTESIAN_POINT('Origin',(0.,0.,7.4));
#15145=CARTESIAN_POINT('',(0.,0.,0.));
#15146=CARTESIAN_POINT('Origin',(0.,0.,0.));
#15147=CARTESIAN_POINT('',(-1.,-1.22464679914735E-16,0.8));
#15148=CARTESIAN_POINT('Origin',(0.,0.,0.8));
#15149=CARTESIAN_POINT('',(-1.,-1.22464679914735E-16,0.));
#15150=CARTESIAN_POINT('',(-1.,-1.22464679914735E-16,0.));
#15151=CARTESIAN_POINT('Origin',(0.,0.,0.));
#15152=CARTESIAN_POINT('Origin',(0.,0.,0.));
#15153=CARTESIAN_POINT('',(-1.7,-2.0818995585505E-16,0.8));
#15154=CARTESIAN_POINT('Origin',(0.,0.,0.8));
#15155=CARTESIAN_POINT('',(-1.7,-2.0818995585505E-16,0.));
#15156=CARTESIAN_POINT('',(-1.7,-2.0818995585505E-16,0.));
#15157=CARTESIAN_POINT('Origin',(0.,0.,0.));
#15158=CARTESIAN_POINT('Origin',(0.,0.,0.8));
#15159=CARTESIAN_POINT('Origin',(0.,0.,0.));
#15160=CARTESIAN_POINT('',(0.,0.,0.));
#15161=CARTESIAN_POINT('Origin',(0.,0.3,2.1));
#15162=CARTESIAN_POINT('',(0.,0.3,2.7));
#15163=CARTESIAN_POINT('',(0.,0.3,2.1));
#15164=CARTESIAN_POINT('',(0.,0.3,2.7));
#15165=CARTESIAN_POINT('',(0.6,0.3,2.7));
#15166=CARTESIAN_POINT('',(0.,0.3,2.7));
#15167=CARTESIAN_POINT('',(0.6,0.3,2.1));
#15168=CARTESIAN_POINT('',(0.6,0.3,2.7));
#15169=CARTESIAN_POINT('',(0.,0.3,2.1));
#15170=CARTESIAN_POINT('Origin',(0.,0.,2.1));
#15171=CARTESIAN_POINT('',(0.,-0.3,2.1));
#15172=CARTESIAN_POINT('Origin',(0.,0.,2.1));
#15173=CARTESIAN_POINT('',(0.6,-0.3,2.1));
#15174=CARTESIAN_POINT('Origin',(0.6,0.,2.1));
#15175=CARTESIAN_POINT('',(0.,-0.3,2.1));
#15176=CARTESIAN_POINT('Origin',(0.,-0.3,2.7));
#15177=CARTESIAN_POINT('',(0.,-0.3,2.7));
#15178=CARTESIAN_POINT('',(0.,-0.3,2.1));
#15179=CARTESIAN_POINT('',(0.6,-0.3,2.7));
#15180=CARTESIAN_POINT('',(0.6,-0.3,2.1));
#15181=CARTESIAN_POINT('',(0.,-0.3,2.7));
#15182=CARTESIAN_POINT('Origin',(0.,2.77555756156289E-17,2.7));
#15183=CARTESIAN_POINT('Origin',(0.,2.77555756156289E-17,2.7));
#15184=CARTESIAN_POINT('Origin',(0.6,2.77555756156289E-17,2.7));
#15185=CARTESIAN_POINT('Origin',(0.6,0.,2.4));
#15186=CARTESIAN_POINT('Origin',(0.,0.,2.4));
#15187=CARTESIAN_POINT('',(0.,0.,0.));
#15188=CARTESIAN_POINT('Origin',(0.,0.,0.));
#15189=CARTESIAN_POINT('',(-1.,-1.22464679914735E-16,1.));
#15190=CARTESIAN_POINT('Origin',(0.,0.,1.));
#15191=CARTESIAN_POINT('',(-1.,-1.22464679914735E-16,0.));
#15192=CARTESIAN_POINT('',(-1.,-1.22464679914735E-16,0.));
#15193=CARTESIAN_POINT('Origin',(0.,0.,0.));
#15194=CARTESIAN_POINT('Origin',(0.,0.,0.));
#15195=CARTESIAN_POINT('',(-1.7,-2.0818995585505E-16,1.));
#15196=CARTESIAN_POINT('Origin',(0.,0.,1.));
#15197=CARTESIAN_POINT('',(-1.7,-2.0818995585505E-16,0.));
#15198=CARTESIAN_POINT('',(-1.7,-2.0818995585505E-16,0.));
#15199=CARTESIAN_POINT('Origin',(0.,0.,0.));
#15200=CARTESIAN_POINT('Origin',(0.,0.,1.));
#15201=CARTESIAN_POINT('Origin',(0.,0.,0.));
#15202=CARTESIAN_POINT('',(0.,0.,0.));
#15203=CARTESIAN_POINT('Origin',(0.,0.,11.2));
#15204=CARTESIAN_POINT('',(-1.,-1.22464679914735E-16,11.4));
#15205=CARTESIAN_POINT('Origin',(0.,0.,11.4));
#15206=CARTESIAN_POINT('',(-1.,-1.22464679914735E-16,11.2));
#15207=CARTESIAN_POINT('',(-1.,-1.22464679914735E-16,11.2));
#15208=CARTESIAN_POINT('Origin',(0.,0.,11.2));
#15209=CARTESIAN_POINT('Origin',(0.,0.,11.2));
#15210=CARTESIAN_POINT('',(-1.5,-1.83697019872103E-16,11.4));
#15211=CARTESIAN_POINT('Origin',(0.,0.,11.4));
#15212=CARTESIAN_POINT('',(-1.5,-1.83697019872103E-16,11.2));
#15213=CARTESIAN_POINT('',(-1.5,-1.83697019872103E-16,11.2));
#15214=CARTESIAN_POINT('Origin',(0.,0.,11.2));
#15215=CARTESIAN_POINT('Origin',(0.,0.,11.4));
#15216=CARTESIAN_POINT('Origin',(0.,0.,11.2));
#15217=CARTESIAN_POINT('',(0.,0.,0.));
#15218=CARTESIAN_POINT('Origin',(0.,0.,11.4));
#15219=CARTESIAN_POINT('',(-1.1,-1.34711147906209E-16,11.6));
#15220=CARTESIAN_POINT('Origin',(0.,0.,11.6));
#15221=CARTESIAN_POINT('',(-1.1,-1.34711147906209E-16,11.4));
#15222=CARTESIAN_POINT('',(-1.1,-1.34711147906209E-16,11.4));
#15223=CARTESIAN_POINT('Origin',(0.,0.,11.4));
#15224=CARTESIAN_POINT('Origin',(0.,0.,11.4));
#15225=CARTESIAN_POINT('',(-1.7,-2.0818995585505E-16,11.6));
#15226=CARTESIAN_POINT('Origin',(0.,0.,11.6));
#15227=CARTESIAN_POINT('',(-1.7,-2.0818995585505E-16,11.4));
#15228=CARTESIAN_POINT('',(-1.7,-2.0818995585505E-16,11.4));
#15229=CARTESIAN_POINT('Origin',(0.,0.,11.4));
#15230=CARTESIAN_POINT('Origin',(0.,0.,11.6));
#15231=CARTESIAN_POINT('Origin',(0.,0.,11.4));
#15232=CARTESIAN_POINT('',(0.,0.,0.));
#15233=CARTESIAN_POINT('Origin',(0.,0.,0.));
#15234=CARTESIAN_POINT('',(-1.,-1.22464679914735E-16,0.2));
#15235=CARTESIAN_POINT('Origin',(0.,0.,0.2));
#15236=CARTESIAN_POINT('',(-1.,-1.22464679914735E-16,0.));
#15237=CARTESIAN_POINT('',(-1.,-1.22464679914735E-16,0.));
#15238=CARTESIAN_POINT('Origin',(0.,0.,0.));
#15239=CARTESIAN_POINT('Origin',(0.,0.,0.));
#15240=CARTESIAN_POINT('',(-1.4,-1.71450551880629E-16,0.2));
#15241=CARTESIAN_POINT('Origin',(0.,0.,0.2));
#15242=CARTESIAN_POINT('',(-1.4,-1.71450551880629E-16,0.));
#15243=CARTESIAN_POINT('',(-1.4,-1.71450551880629E-16,0.));
#15244=CARTESIAN_POINT('Origin',(0.,0.,0.));
#15245=CARTESIAN_POINT('Origin',(0.,0.,0.2));
#15246=CARTESIAN_POINT('Origin',(0.,0.,0.));
#15247=CARTESIAN_POINT('',(0.,0.,0.));
#15248=CARTESIAN_POINT('Origin',(-0.1,0.,0.1));
#15249=CARTESIAN_POINT('',(-0.1,0.894427190999916,0.));
#15250=CARTESIAN_POINT('',(-0.1,0.894427190999916,0.1));
#15251=CARTESIAN_POINT('',(-0.1,0.894427190999916,0.));
#15252=CARTESIAN_POINT('',(-0.1,1.39642400437689,0.));
#15253=CARTESIAN_POINT('',(-0.1,0.,0.));
#15254=CARTESIAN_POINT('',(-0.1,1.39642400437689,0.1));
#15255=CARTESIAN_POINT('',(-0.1,1.39642400437689,0.));
#15256=CARTESIAN_POINT('',(-0.1,0.,0.1));
#15257=CARTESIAN_POINT('Origin',(0.1,2.8,0.1));
#15258=CARTESIAN_POINT('',(0.1,0.894427190999916,0.1));
#15259=CARTESIAN_POINT('',(0.1,0.894427190999916,0.));
#15260=CARTESIAN_POINT('',(0.1,0.894427190999916,0.));
#15261=CARTESIAN_POINT('',(0.1,1.39642400437689,0.1));
#15262=CARTESIAN_POINT('',(0.1,1.4,0.1));
#15263=CARTESIAN_POINT('',(0.1,1.39642400437689,0.));
#15264=CARTESIAN_POINT('',(0.1,1.39642400437689,0.));
#15265=CARTESIAN_POINT('',(0.1,1.4,0.));
#15266=CARTESIAN_POINT('Origin',(0.,0.,0.));
#15267=CARTESIAN_POINT('Origin',(0.,0.,0.));
#15268=CARTESIAN_POINT('Origin',(0.,0.,0.));
#15269=CARTESIAN_POINT('Origin',(0.,0.,0.));
#15270=CARTESIAN_POINT('Origin',(0.,0.,0.1));
#15271=CARTESIAN_POINT('Origin',(0.,0.,0.));
#15272=CARTESIAN_POINT('Origin',(0.,0.,0.1));
#15273=CARTESIAN_POINT('Origin',(0.,0.,0.1));
#15274=CARTESIAN_POINT('',(0.,0.,0.));
#15275=CARTESIAN_POINT('Origin',(0.,0.,0.));
#15276=CARTESIAN_POINT('',(-0.294573206171349,0.000178211181277831,12.832217611709));
#15277=CARTESIAN_POINT('',(-0.294456685750782,0.000237168791136358,12.817782388291));
#15278=CARTESIAN_POINT('',(-0.2942,-3.60291088309151E-17,0.));
#15279=CARTESIAN_POINT('',(0.129212637845014,0.2648431347106,12.8));
#15280=CARTESIAN_POINT('Ctrl Pts',(-0.294573206171349,0.000178211181277831,
12.832217611709));
#15281=CARTESIAN_POINT('Ctrl Pts',(-0.294638639138964,0.00983177811479042,
12.8316935247725));
#15282=CARTESIAN_POINT('Ctrl Pts',(-0.294205630785965,0.0194791637026875,
12.831169437836));
#15283=CARTESIAN_POINT('Ctrl Pts',(-0.293254985022131,0.029074932121012,
12.8306453508995));
#15284=CARTESIAN_POINT('Ctrl Pts',(-0.283645993540782,0.126067587531217,
12.8253479550661));
#15285=CARTESIAN_POINT('Ctrl Pts',(-0.221150622395202,0.217786580006569,
12.8200505592328));
#15286=CARTESIAN_POINT('Ctrl Pts',(-0.134385324348696,0.262257101239527,
12.8147531633995));
#15287=CARTESIAN_POINT('Ctrl Pts',(-0.0538386645837653,0.303540333406841,
12.8098354422663));
#15288=CARTESIAN_POINT('Ctrl Pts',(0.0476236474357998,0.304105165469236,
12.8049177211331));
#15289=CARTESIAN_POINT('Ctrl Pts',(0.129215683241976,0.264846751495055,
12.8));
#15290=CARTESIAN_POINT('',(-0.2942,-3.60291088309151E-17,12.8));
#15291=CARTESIAN_POINT('Origin',(0.,0.,12.8));
#15292=CARTESIAN_POINT('',(-0.2942,3.60291088309151E-17,0.));
#15293=CARTESIAN_POINT('',(-0.2942,-3.60291088309151E-17,0.));
#15294=CARTESIAN_POINT('Origin',(0.,0.,0.));
#15295=CARTESIAN_POINT('',(-0.128892185405308,0.264462557919725,12.8));
#15296=CARTESIAN_POINT('Origin',(0.,0.,12.8));
#15297=CARTESIAN_POINT('Ctrl Pts',(-0.128892185405307,0.264462557919724,
12.8));
#15298=CARTESIAN_POINT('Ctrl Pts',(-0.217043456109747,0.22149991694429,
12.8053049893273));
#15299=CARTESIAN_POINT('Ctrl Pts',(-0.281220970323085,0.131282598258039,
12.8106099786547));
#15300=CARTESIAN_POINT('Ctrl Pts',(-0.292601064222616,0.0344997435524954,
12.815914967982));
#15301=CARTESIAN_POINT('Ctrl Pts',(-0.293936374384136,0.0231434990003663,
12.8165374414184));
#15302=CARTESIAN_POINT('Ctrl Pts',(-0.294544766717762,0.0116968597821011,
12.8171599148547));
#15303=CARTESIAN_POINT('Ctrl Pts',(-0.294456685750782,0.000237168791136358,
12.817782388291));
#15304=CARTESIAN_POINT('Origin',(0.,0.,0.));
#15305=CARTESIAN_POINT('',(-0.293819506992835,0.000164351555994161,12.932217611709));
#15306=CARTESIAN_POINT('',(-0.293800895129206,0.000154060581779477,12.917782388291));
#15307=CARTESIAN_POINT('',(-0.2942,-3.60291088309151E-17,0.));
#15308=CARTESIAN_POINT('Ctrl Pts',(-0.293819506992835,0.000164351555994161,
12.932217611709));
#15309=CARTESIAN_POINT('Ctrl Pts',(-0.294014132231746,0.0386044236212459,
12.9301445664391));
#15310=CARTESIAN_POINT('Ctrl Pts',(-0.287011791888666,0.0769763465444152,
12.9280715211693));
#15311=CARTESIAN_POINT('Ctrl Pts',(-0.272482130953542,0.112247367194594,
12.9259984758995));
#15312=CARTESIAN_POINT('Ctrl Pts',(-0.235353484311062,0.202377843623973,
12.9207010800661));
#15313=CARTESIAN_POINT('Ctrl Pts',(-0.149072102201679,0.272259703394973,
12.9154036842328));
#15314=CARTESIAN_POINT('Ctrl Pts',(-0.0531946070450342,0.28985545356503,
12.9101062883995));
#15315=CARTESIAN_POINT('Ctrl Pts',(0.042682888111611,0.307451203735087,
12.9048088925661));
#15316=CARTESIAN_POINT('Ctrl Pts',(0.148156496315518,0.2727608443042,12.8995114967328));
#15317=CARTESIAN_POINT('Ctrl Pts',(0.214869204494931,0.201686733123392,
12.8942141008995));
#15318=CARTESIAN_POINT('Ctrl Pts',(0.281581912674343,0.130612621942583,
12.8889167050661));
#15319=CARTESIAN_POINT('Ctrl Pts',(0.30953372082926,0.0231547590118516,
12.8836193092328));
#15320=CARTESIAN_POINT('Ctrl Pts',(0.285911633440566,-0.0714169606488347,
12.8783219133995));
#15321=CARTESIAN_POINT('Ctrl Pts',(0.262289546051872,-0.165988680309521,
12.8730245175661));
#15322=CARTESIAN_POINT('Ctrl Pts',(0.187093563119567,-0.247674256700163,
12.8677271217328));
#15323=CARTESIAN_POINT('Ctrl Pts',(0.0947944415992507,-0.279032132710234,
12.8624297258995));
#15324=CARTESIAN_POINT('Ctrl Pts',(0.00249532007893488,-0.310390008720306,
12.8571323300661));
#15325=CARTESIAN_POINT('Ctrl Pts',(-0.106906940029391,-0.291420184349807,
12.8518349342328));
#15326=CARTESIAN_POINT('Ctrl Pts',(-0.183246764174995,-0.230802112992029,
12.8465375383995));
#15327=CARTESIAN_POINT('Ctrl Pts',(-0.252034065188834,-0.176181165563425,
12.8417642295026));
#15328=CARTESIAN_POINT('Ctrl Pts',(-0.293977252056274,-0.0877450964243544,
12.8369909206058));
#15329=CARTESIAN_POINT('Ctrl Pts',(-0.294573206171349,0.000178211181277831,
12.832217611709));
#15330=CARTESIAN_POINT('Ctrl Pts',(-0.294456685750782,0.000237168791136358,
12.817782388291));
#15331=CARTESIAN_POINT('Ctrl Pts',(-0.293794102412292,-0.0859676104622492,
12.822464904182));
#15332=CARTESIAN_POINT('Ctrl Pts',(-0.253720165912887,-0.172910950724067,
12.827147420073));
#15333=CARTESIAN_POINT('Ctrl Pts',(-0.18719426584733,-0.227670130650132,
12.831829935964));
#15334=CARTESIAN_POINT('Ctrl Pts',(-0.111824699986792,-0.289708759422378,
12.8371349252914));
#15335=CARTESIAN_POINT('Ctrl Pts',(-0.00250289467999464,-0.310437626242033,
12.8424399146187));
#15336=CARTESIAN_POINT('Ctrl Pts',(0.0904196621835738,-0.280470963636124,
12.847744903946));
#15337=CARTESIAN_POINT('Ctrl Pts',(0.183342219047142,-0.250504301030214,
12.8530498932734));
#15338=CARTESIAN_POINT('Ctrl Pts',(0.259865527467481,-0.169842108998739,
12.8583548826007));
#15339=CARTESIAN_POINT('Ctrl Pts',(0.284861830842183,-0.0754928832674847,
12.863659871928));
#15340=CARTESIAN_POINT('Ctrl Pts',(0.309858134216885,0.0188563424637699,
12.8689648612554));
#15341=CARTESIAN_POINT('Ctrl Pts',(0.28332743254595,0.126892601894804,12.8742698505827));
#15342=CARTESIAN_POINT('Ctrl Pts',(0.217441929334565,0.198921329027957,
12.8795748399101));
#15343=CARTESIAN_POINT('Ctrl Pts',(0.151556426123181,0.270950056161109,
12.8848798292374));
#15344=CARTESIAN_POINT('Ctrl Pts',(0.0463161213713476,0.30697125099638,
12.8901848185647));
#15345=CARTESIAN_POINT('Ctrl Pts',(-0.0498919590377675,0.290443329283603,
12.8954898078921));
#15346=CARTESIAN_POINT('Ctrl Pts',(-0.146100039446882,0.273915407570827,
12.9007947972194));
#15347=CARTESIAN_POINT('Ctrl Pts',(-0.233275895513279,0.204838369310003,
12.9060997865467));
#15348=CARTESIAN_POINT('Ctrl Pts',(-0.271352858586062,0.114956956369256,
12.9114047758741));
#15349=CARTESIAN_POINT('Ctrl Pts',(-0.286611457457756,0.0789387365479301,
12.9135306466797));
#15350=CARTESIAN_POINT('Ctrl Pts',(-0.29398551548852,0.0395796482908291,
12.9156565174854));
#15351=CARTESIAN_POINT('Ctrl Pts',(-0.293800895129206,0.000154060581779477,
12.917782388291));
#15352=CARTESIAN_POINT('Origin',(0.,0.,0.));
#15353=CARTESIAN_POINT('',(-0.293978383054635,-0.000241987351228545,13.032217611709));
#15354=CARTESIAN_POINT('',(-0.293977558237541,-0.000244103523127173,13.017782388291));
#15355=CARTESIAN_POINT('',(-0.2942,-3.60291088309151E-17,0.));
#15356=CARTESIAN_POINT('Ctrl Pts',(-0.293978383054635,-0.000241987351228545,
13.032217611709));
#15357=CARTESIAN_POINT('Ctrl Pts',(-0.293459536795742,0.0668289020834338,
13.0285956081058));
#15358=CARTESIAN_POINT('Ctrl Pts',(-0.270690894883612,0.134218310941281,
13.0249736045026));
#15359=CARTESIAN_POINT('Ctrl Pts',(-0.22864087855502,0.18592830985058,13.0213516008995));
#15360=CARTESIAN_POINT('Ctrl Pts',(-0.167140227065884,0.261557260778287,
13.0160542050661));
#15361=CARTESIAN_POINT('Ctrl Pts',(-0.0643951667298436,0.303646694219936,
13.0107568092328));
#15362=CARTESIAN_POINT('Ctrl Pts',(0.0324891899508726,0.292900047757626,
13.0054594133995));
#15363=CARTESIAN_POINT('Ctrl Pts',(0.129373546631589,0.282153401295317,
13.0001620175661));
#15364=CARTESIAN_POINT('Ctrl Pts',(0.220397199656981,0.218570674929048,
12.9948646217328));
#15365=CARTESIAN_POINT('Ctrl Pts',(0.263828885312461,0.131302362204768,
12.9895672258995));
#15366=CARTESIAN_POINT('Ctrl Pts',(0.307260570967942,0.0440340494804873,
12.9842698300661));
#15367=CARTESIAN_POINT('Ctrl Pts',(0.30310028925351,-0.0669198496018051,
12.9789724342328));
#15368=CARTESIAN_POINT('Ctrl Pts',(0.253255413164487,-0.150690690040053,
12.9736750383995));
#15369=CARTESIAN_POINT('Ctrl Pts',(0.203410537075464,-0.2344615304783,12.9683776425661));
#15370=CARTESIAN_POINT('Ctrl Pts',(0.10788106661185,-0.291049312272503,
12.9630802467328));
#15371=CARTESIAN_POINT('Ctrl Pts',(0.0104639653641406,-0.294510570060203,
12.9577828508995));
#15372=CARTESIAN_POINT('Ctrl Pts',(-0.0869531358835682,-0.297971827847904,
12.9524854550661));
#15373=CARTESIAN_POINT('Ctrl Pts',(-0.186257867915372,-0.248306561629102,
12.9471880592328));
#15374=CARTESIAN_POINT('Ctrl Pts',(-0.241922278343485,-0.168284381975822,
12.9418906633995));
#15375=CARTESIAN_POINT('Ctrl Pts',(-0.275803373654782,-0.119577513889043,
12.938666312836));
#15376=CARTESIAN_POINT('Ctrl Pts',(-0.29351679290941,-0.0596241488826022,
12.9354419622725));
#15377=CARTESIAN_POINT('Ctrl Pts',(-0.293819506992835,0.000164351555994161,
12.932217611709));
#15378=CARTESIAN_POINT('Ctrl Pts',(-0.293800895129206,0.000154060581779477,
12.917782388291));
#15379=CARTESIAN_POINT('Ctrl Pts',(-0.293524805913338,-0.0588046568438365,
12.9209615068127));
#15380=CARTESIAN_POINT('Ctrl Pts',(-0.276344869041408,-0.117912090294522,
12.9241406253344));
#15381=CARTESIAN_POINT('Ctrl Pts',(-0.243350877161725,-0.166217658514054,
12.9273197438561));
#15382=CARTESIAN_POINT('Ctrl Pts',(-0.188293862585438,-0.246825072835943,
12.9326247331834));
#15383=CARTESIAN_POINT('Ctrl Pts',(-0.0892017633536947,-0.29735411385905,
12.9379297225108));
#15384=CARTESIAN_POINT('Ctrl Pts',(0.00837448788296055,-0.294579959740858,
12.9432347118381));
#15385=CARTESIAN_POINT('Ctrl Pts',(0.105950739119616,-0.291805805622667,
12.9485397011654));
#15386=CARTESIAN_POINT('Ctrl Pts',(0.202011142361183,-0.235728456363176,
12.9538446904928));
#15387=CARTESIAN_POINT('Ctrl Pts',(0.252400245841885,-0.152124079723166,
12.9591496798201));
#15388=CARTESIAN_POINT('Ctrl Pts',(0.302789349322588,-0.068519703083155,
12.9644546691475));
#15389=CARTESIAN_POINT('Ctrl Pts',(0.307507153042424,0.0426117009373751,
12.9697596584748));
#15390=CARTESIAN_POINT('Ctrl Pts',(0.264384723644278,0.130185938245225,
12.9750646478021));
#15391=CARTESIAN_POINT('Ctrl Pts',(0.221262294246132,0.217760175553074,
12.9803696371295));
#15392=CARTESIAN_POINT('Ctrl Pts',(0.130299631730003,0.281777246148244,
12.9856746264568));
#15393=CARTESIAN_POINT('Ctrl Pts',(0.0333096771051611,0.292810643338737,
12.9909796157841));
#15394=CARTESIAN_POINT('Ctrl Pts',(-0.0636802775196813,0.303844040529229,
12.9962846051115));
#15395=CARTESIAN_POINT('Ctrl Pts',(-0.166697524253236,0.261893764315045,
13.0015895944388));
#15396=CARTESIAN_POINT('Ctrl Pts',(-0.228388209822111,0.186242989953447,
13.0068945837661));
#15397=CARTESIAN_POINT('Ctrl Pts',(-0.270592261142874,0.134488513014659,
13.0105238519411));
#15398=CARTESIAN_POINT('Ctrl Pts',(-0.293454446900826,0.0669613589840213,
13.0141531201161));
#15399=CARTESIAN_POINT('Ctrl Pts',(-0.293977558237541,-0.000244103523127173,
13.017782388291));
#15400=CARTESIAN_POINT('Origin',(0.,0.,0.));
#15401=CARTESIAN_POINT('',(-0.294688566460017,-4.3425772024458E-5,13.132217611709));
#15402=CARTESIAN_POINT('',(-0.294684770789603,-5.92838055088064E-5,13.117782388291));
#15403=CARTESIAN_POINT('',(-0.2942,-3.60291088309151E-17,0.));
#15404=CARTESIAN_POINT('Ctrl Pts',(-0.294688566460017,-4.3425772024458E-5,
13.132217611709));
#15405=CARTESIAN_POINT('Ctrl Pts',(-0.294492695162095,0.0951154314666305,
13.1270466497725));
#15406=CARTESIAN_POINT('Ctrl Pts',(-0.244188233801183,0.190452094564122,
13.121875687836));
#15407=CARTESIAN_POINT('Ctrl Pts',(-0.165446572490844,0.243871726854215,
13.1167047258995));
#15408=CARTESIAN_POINT('Ctrl Pts',(-0.0847796185164032,0.298597509210938,
13.1114073300661));
#15409=CARTESIAN_POINT('Ctrl Pts',(0.0257321580046905,0.309331395447293,
13.1061099342328));
#15410=CARTESIAN_POINT('Ctrl Pts',(0.115422863317555,0.271152263674646,
13.1008125383995));
#15411=CARTESIAN_POINT('Ctrl Pts',(0.205113568630419,0.232973131901999,
13.0955151425661));
#15412=CARTESIAN_POINT('Ctrl Pts',(0.273983202735053,0.145880982120351,
13.0902177467328));
#15413=CARTESIAN_POINT('Ctrl Pts',(0.290457378744519,0.049804604878551,
13.0849203508995));
#15414=CARTESIAN_POINT('Ctrl Pts',(0.306931554753985,-0.0462717723632486,
13.0796229550661));
#15415=CARTESIAN_POINT('Ctrl Pts',(0.271010272668282,-0.1513323770652,13.0743255592328));
#15416=CARTESIAN_POINT('Ctrl Pts',(0.19916221987775,-0.217210491733346,
13.0690281633995));
#15417=CARTESIAN_POINT('Ctrl Pts',(0.127314167087218,-0.283088606401493,
13.0637307675661));
#15418=CARTESIAN_POINT('Ctrl Pts',(0.0195393435918585,-0.309784231035834,
13.0584333717328));
#15419=CARTESIAN_POINT('Ctrl Pts',(-0.0747511573933412,-0.285058330392084,
13.0531359758995));
#15420=CARTESIAN_POINT('Ctrl Pts',(-0.169041658378541,-0.260332429748335,
13.0478385800661));
#15421=CARTESIAN_POINT('Ctrl Pts',(-0.24984783685358,-0.184185003826495,
13.0425411842328));
#15422=CARTESIAN_POINT('Ctrl Pts',(-0.280122804769983,-0.0915270566586923,
13.0372437883995));
#15423=CARTESIAN_POINT('Ctrl Pts',(-0.289697782289419,-0.0622223927007149,
13.0355683961693));
#15424=CARTESIAN_POINT('Ctrl Pts',(-0.294218380328531,-0.0312662654416913,
13.0338930039391));
#15425=CARTESIAN_POINT('Ctrl Pts',(-0.293978383054635,-0.000241987351228545,
13.032217611709));
#15426=CARTESIAN_POINT('Ctrl Pts',(-0.293977558237541,-0.000244103523127173,
13.017782388291));
#15427=CARTESIAN_POINT('Ctrl Pts',(-0.294219091430933,-0.0312744957809374,
13.0194581094434));
#15428=CARTESIAN_POINT('Ctrl Pts',(-0.289698173215612,-0.0622363068513482,
13.0211338305958));
#15429=CARTESIAN_POINT('Ctrl Pts',(-0.280119774337342,-0.091545292928116,
13.0228095517481));
#15430=CARTESIAN_POINT('Ctrl Pts',(-0.249796528879502,-0.184331528939066,
13.0281145410755));
#15431=CARTESIAN_POINT('Ctrl Pts',(-0.168785913559629,-0.260552728451954,
13.0334195304028));
#15432=CARTESIAN_POINT('Ctrl Pts',(-0.0743260837926121,-0.285172326966721,
13.0387245197302));
#15433=CARTESIAN_POINT('Ctrl Pts',(0.0201337459744046,-0.309791925481488,
13.0440295090575));
#15434=CARTESIAN_POINT('Ctrl Pts',(0.128042790188565,-0.282809922998135,
13.0493344983848));
#15435=CARTESIAN_POINT('Ctrl Pts',(0.199798520936279,-0.216629121303023,
13.0546394877122));
#15436=CARTESIAN_POINT('Ctrl Pts',(0.271554251683993,-0.150448319607911,
13.0599444770395));
#15437=CARTESIAN_POINT('Ctrl Pts',(0.307156668965259,-0.0450687187010392,
13.0652494663668));
#15438=CARTESIAN_POINT('Ctrl Pts',(0.290240410451035,0.0510698486205661,
13.0705544556942));
#15439=CARTESIAN_POINT('Ctrl Pts',(0.273324151936811,0.147208415942171,
13.0758594450215));
#15440=CARTESIAN_POINT('Ctrl Pts',(0.203889217627098,0.23410594967851,13.0811644343489));
#15441=CARTESIAN_POINT('Ctrl Pts',(0.113852756432599,0.271818274816414,
13.0864694236762));
#15442=CARTESIAN_POINT('Ctrl Pts',(0.0238162952380993,0.309530599954319,
13.0917744130035));
#15443=CARTESIAN_POINT('Ctrl Pts',(-0.0868216928411871,0.29805771649379,
13.0970794023309));
#15444=CARTESIAN_POINT('Ctrl Pts',(-0.16720425947304,0.242673361913228,
13.1023843916582));
#15445=CARTESIAN_POINT('Ctrl Pts',(-0.244975731695611,0.189088076268463,
13.1075170572025));
#15446=CARTESIAN_POINT('Ctrl Pts',(-0.294425452342338,0.09439776822128,
13.1126497227468));
#15447=CARTESIAN_POINT('Ctrl Pts',(-0.294684770789603,-5.92838055088064E-5,
13.117782388291));
#15448=CARTESIAN_POINT('Origin',(0.,0.,0.));
#15449=CARTESIAN_POINT('',(-0.294107431028703,0.000266555779104893,13.232217611709));
#15450=CARTESIAN_POINT('',(-0.294157826435532,0.000271978496102963,13.217782388291));
#15451=CARTESIAN_POINT('',(-0.2942,-3.60291088309151E-17,0.));
#15452=CARTESIAN_POINT('Ctrl Pts',(-0.294107431028703,0.000266555779104893,
13.232217611709));
#15453=CARTESIAN_POINT('Ctrl Pts',(-0.294339337791913,0.026579066670166,
13.2307950872725));
#15454=CARTESIAN_POINT('Ctrl Pts',(-0.29110065943816,0.0528354654390751,
13.229372562836));
#15455=CARTESIAN_POINT('Ctrl Pts',(-0.28416559484468,0.0780762592101134,
13.2279500383995));
#15456=CARTESIAN_POINT('Ctrl Pts',(-0.258339829508931,0.172071464017823,
13.2226526425661));
#15457=CARTESIAN_POINT('Ctrl Pts',(-0.181253577517488,0.251982532843938,
13.2173552467328));
#15458=CARTESIAN_POINT('Ctrl Pts',(-0.0882482661206186,0.281172955778023,
13.2120578508995));
#15459=CARTESIAN_POINT('Ctrl Pts',(0.00475704527625133,0.310363378712107,
13.2067604550661));
#15460=CARTESIAN_POINT('Ctrl Pts',(0.113681416078549,0.288833155754161,
13.2014630592328));
#15461=CARTESIAN_POINT('Ctrl Pts',(0.1885867242503,0.226453162726531,13.1961656633995));
#15462=CARTESIAN_POINT('Ctrl Pts',(0.263492032422051,0.164073169698901,
13.1908682675661));
#15463=CARTESIAN_POINT('Ctrl Pts',(0.304378277963256,0.0608434066015877,
13.1855708717328));
#15464=CARTESIAN_POINT('Ctrl Pts',(0.292500506687337,-0.035908788554837,
13.1802734758995));
#15465=CARTESIAN_POINT('Ctrl Pts',(0.280622735411417,-0.132660983711262,
13.1749760800661));
#15466=CARTESIAN_POINT('Ctrl Pts',(0.215980947318375,-0.222935610926797,
13.1696786842328));
#15467=CARTESIAN_POINT('Ctrl Pts',(0.128211205478304,-0.265344821495433,
13.1643812883995));
#15468=CARTESIAN_POINT('Ctrl Pts',(0.0404414636382319,-0.307754032064069,
13.1590838925661));
#15469=CARTESIAN_POINT('Ctrl Pts',(-0.0704562319488692,-0.302297825985805,
13.1537864967328));
#15470=CARTESIAN_POINT('Ctrl Pts',(-0.153639056706568,-0.251477688371532,
13.1484891008995));
#15471=CARTESIAN_POINT('Ctrl Pts',(-0.236821881464266,-0.200657550757259,
13.1431917050661));
#15472=CARTESIAN_POINT('Ctrl Pts',(-0.292289835392562,-0.104473481606977,
13.1378943092328));
#15473=CARTESIAN_POINT('Ctrl Pts',(-0.294612746642817,-0.00702260779328966,
13.1325969133995));
#15474=CARTESIAN_POINT('Ctrl Pts',(-0.294668187982413,-0.0046967303029458,
13.1324704795026));
#15475=CARTESIAN_POINT('Ctrl Pts',(-0.294693355660127,-0.00237013118713854,
13.1323440456058));
#15476=CARTESIAN_POINT('Ctrl Pts',(-0.294688566460017,-4.3425772024458E-5,
13.132217611709));
#15477=CARTESIAN_POINT('Ctrl Pts',(-0.294684770789603,-5.92838055088064E-5,
13.117782388291));
#15478=CARTESIAN_POINT('Ctrl Pts',(-0.294693477130483,-0.00323057879859576,
13.1179547120741));
#15479=CARTESIAN_POINT('Ctrl Pts',(-0.294646735599431,-0.00640161086335999,
13.1181270358572));
#15480=CARTESIAN_POINT('Ctrl Pts',(-0.294543756425539,-0.00957081555894318,
13.1182993596402));
#15481=CARTESIAN_POINT('Ctrl Pts',(-0.291373541561766,-0.107134812749959,
13.1236043489676));
#15482=CARTESIAN_POINT('Ctrl Pts',(-0.234905966649797,-0.202966981431395,
13.1289093382949));
#15483=CARTESIAN_POINT('Ctrl Pts',(-0.151097474548945,-0.253016161695952,
13.1342143276222));
#15484=CARTESIAN_POINT('Ctrl Pts',(-0.0672889824480926,-0.303065341960509,
13.1395193169496));
#15485=CARTESIAN_POINT('Ctrl Pts',(0.0438604268416431,-0.307331533808189,
13.1448243062769));
#15486=CARTESIAN_POINT('Ctrl Pts',(0.131258719251342,-0.26385369724767,
13.1501292956042));
#15487=CARTESIAN_POINT('Ctrl Pts',(0.218657011661041,-0.220375860687151,
13.1554342849316));
#15488=CARTESIAN_POINT('Ctrl Pts',(0.282304187190703,-0.129153995718433,
13.1607392742589));
#15489=CARTESIAN_POINT('Ctrl Pts',(0.292943557088177,-0.0321200449435113,
13.1660442635862));
#15490=CARTESIAN_POINT('Ctrl Pts',(0.30358292698565,0.0649139058314107,
13.1713492529136));
#15491=CARTESIAN_POINT('Ctrl Pts',(0.261214491250936,0.167759942412537,
13.1766542422409));
#15492=CARTESIAN_POINT('Ctrl Pts',(0.18531374311845,0.229142840892087,13.1819592315683));
#15493=CARTESIAN_POINT('Ctrl Pts',(0.109412994985964,0.290525739371636,
13.1872642208956));
#15494=CARTESIAN_POINT('Ctrl Pts',(-2.00655442916947E-5,0.31044549974961,
13.1925692102229));
#15495=CARTESIAN_POINT('Ctrl Pts',(-0.0926823581075636,0.27974560840399,
13.1978741995503));
#15496=CARTESIAN_POINT('Ctrl Pts',(-0.185344650670836,0.249045717058369,
13.2031791888776));
#15497=CARTESIAN_POINT('Ctrl Pts',(-0.261236175267123,0.167726173989153,
13.2084841782049));
#15498=CARTESIAN_POINT('Ctrl Pts',(-0.285471884901514,0.0731671227495215,
13.2137891675323));
#15499=CARTESIAN_POINT('Ctrl Pts',(-0.291552860931422,0.0494413341230131,
13.2151202411185));
#15500=CARTESIAN_POINT('Ctrl Pts',(-0.294381808637396,0.0248820429063915,
13.2164513147048));
#15501=CARTESIAN_POINT('Ctrl Pts',(-0.294157826435532,0.000271978496102963,
13.217782388291));
#15502=CARTESIAN_POINT('Origin',(0.,0.,0.));
#15503=CARTESIAN_POINT('',(-0.293756705318437,-9.65891231691218E-5,13.332217611709));
#15504=CARTESIAN_POINT('',(-0.293733177601347,-5.56197620117739E-5,13.317782388291));
#15505=CARTESIAN_POINT('',(-0.2942,-3.60291088309151E-17,0.));
#15506=CARTESIAN_POINT('Ctrl Pts',(-0.293756705318437,-9.65891231691218E-5,
13.332217611709));
#15507=CARTESIAN_POINT('Ctrl Pts',(-0.29359459382837,0.0550324553525043,
13.3292461289391));
#15508=CARTESIAN_POINT('Ctrl Pts',(-0.27871547764323,0.110242707595751,
13.3262746461693));
#15509=CARTESIAN_POINT('Ctrl Pts',(-0.249665643167405,0.156566455486698,
13.3233031633995));
#15510=CARTESIAN_POINT('Ctrl Pts',(-0.197877198127916,0.23914988203496,
13.3180057675661));
#15511=CARTESIAN_POINT('Ctrl Pts',(-0.101051667078895,0.29349040285122,
13.3127083717328));
#15512=CARTESIAN_POINT('Ctrl Pts',(-0.0035803010767538,0.294674689259135,
13.3074109758995));
#15513=CARTESIAN_POINT('Ctrl Pts',(0.093891064925387,0.295858975667049,
13.3021135800661));
#15514=CARTESIAN_POINT('Ctrl Pts',(0.192008265880649,0.243887027666619,
13.2968161842328));
#15515=CARTESIAN_POINT('Ctrl Pts',(0.245787916885835,0.162586239740655,
13.2915187883995));
#15516=CARTESIAN_POINT('Ctrl Pts',(0.299567567891021,0.081285451814691,
13.2862213925661));
#15517=CARTESIAN_POINT('Ctrl Pts',(0.30900966894613,-0.0293441760368059,
13.2809239967328));
#15518=CARTESIAN_POINT('Ctrl Pts',(0.269785329248371,-0.118582730077581,
13.2756266008995));
#15519=CARTESIAN_POINT('Ctrl Pts',(0.230560989550612,-0.207821284118357,
13.2703292050661));
#15520=CARTESIAN_POINT('Ctrl Pts',(0.142670209099985,-0.275668764348411,
13.2650318092328));
#15521=CARTESIAN_POINT('Ctrl Pts',(0.0464079278430225,-0.291019401563061,
13.2597344133995));
#15522=CARTESIAN_POINT('Ctrl Pts',(-0.0498543534139403,-0.306370038777712,
13.2544370175661));
#15523=CARTESIAN_POINT('Ctrl Pts',(-0.154488135477239,-0.269223832976959,
13.2491396217328));
#15524=CARTESIAN_POINT('Ctrl Pts',(-0.219522387168861,-0.196611059681931,
13.2438422258995));
#15525=CARTESIAN_POINT('Ctrl Pts',(-0.267092810377316,-0.143497196353984,
13.2399673545026));
#15526=CARTESIAN_POINT('Ctrl Pts',(-0.293475730890246,-0.0714071485275604,
13.2360924831058));
#15527=CARTESIAN_POINT('Ctrl Pts',(-0.294107431028703,0.000266555779104893,
13.232217611709));
#15528=CARTESIAN_POINT('Ctrl Pts',(-0.294157826435532,0.000271978496102963,
13.217782388291));
#15529=CARTESIAN_POINT('Ctrl Pts',(-0.293489128320791,-0.0732012865127652,
13.2217563040321));
#15530=CARTESIAN_POINT('Ctrl Pts',(-0.265609085010938,-0.147127102658161,
13.2257302197732));
#15531=CARTESIAN_POINT('Ctrl Pts',(-0.21581576504657,-0.200676806043974,
13.2297041355143));
#15532=CARTESIAN_POINT('Ctrl Pts',(-0.14934404088474,-0.272163124187789,
13.2350091248416));
#15533=CARTESIAN_POINT('Ctrl Pts',(-0.0438206978885843,-0.307337201065372,
13.240314114169));
#15534=CARTESIAN_POINT('Ctrl Pts',(0.0522483628297525,-0.290030573409733,
13.2456191034963));
#15535=CARTESIAN_POINT('Ctrl Pts',(0.14831742354809,-0.272723945754094,
13.2509240928236));
#15536=CARTESIAN_POINT('Ctrl Pts',(0.234932201988608,-0.202936613565231,
13.256229082151));
#15537=CARTESIAN_POINT('Ctrl Pts',(0.272278494649526,-0.112747710601187,
13.2615340714783));
#15538=CARTESIAN_POINT('Ctrl Pts',(0.309624787310445,-0.022558807637142,
13.2668390608057));
#15539=CARTESIAN_POINT('Ctrl Pts',(0.297702594191763,0.0880316661020849,
13.272144050133));
#15540=CARTESIAN_POINT('Ctrl Pts',(0.241992187856524,0.168188602396665,
13.2774490394603));
#15541=CARTESIAN_POINT('Ctrl Pts',(0.186281781521285,0.248345538691245,
13.2827540287877));
#15542=CARTESIAN_POINT('Ctrl Pts',(0.0867831619694888,0.298068937541179,
13.288059018115));
#15543=CARTESIAN_POINT('Ctrl Pts',(-0.0107671528494052,0.294502450563172,
13.2933640074423));
#15544=CARTESIAN_POINT('Ctrl Pts',(-0.108317467668299,0.290935963585165,
13.2986689967697));
#15545=CARTESIAN_POINT('Ctrl Pts',(-0.203919477754291,0.234079590779218,
13.303973986097));
#15546=CARTESIAN_POINT('Ctrl Pts',(-0.253627821392627,0.150068493985587,
13.3092789754243));
#15547=CARTESIAN_POINT('Ctrl Pts',(-0.280187131430457,0.105181124923475,
13.3121134463799));
#15548=CARTESIAN_POINT('Ctrl Pts',(-0.293644738529364,0.052541637658281,
13.3149479173355));
#15549=CARTESIAN_POINT('Ctrl Pts',(-0.293733177601347,-5.56197620117739E-5,
13.317782388291));
#15550=CARTESIAN_POINT('Origin',(0.,0.,0.));
#15551=CARTESIAN_POINT('',(-0.294460332090693,-0.000220795745557084,13.432217611709));
#15552=CARTESIAN_POINT('',(-0.294362671296069,-0.000253937998619662,13.417782388291));
#15553=CARTESIAN_POINT('',(-0.2942,-3.60291088309151E-17,0.));
#15554=CARTESIAN_POINT('Ctrl Pts',(-0.294460332090693,-0.000220795745557084,
13.432217611709));
#15555=CARTESIAN_POINT('Ctrl Pts',(-0.293757341683982,0.0831358178453026,
13.4276971706058));
#15556=CARTESIAN_POINT('Ctrl Pts',(-0.25664007441063,0.167036070084589,
13.4231767295026));
#15557=CARTESIAN_POINT('Ctrl Pts',(-0.194033810233309,0.221803347340193,
13.4186562883995));
#15558=CARTESIAN_POINT('Ctrl Pts',(-0.120667040171587,0.285983797812974,
13.4133588925661));
#15559=CARTESIAN_POINT('Ctrl Pts',(-0.0122964079182814,0.310156136338401,
13.4080614967328));
#15560=CARTESIAN_POINT('Ctrl Pts',(0.0813910654447742,0.283234545604937,
13.4027641008995));
#15561=CARTESIAN_POINT('Ctrl Pts',(0.17507853880783,0.256312954871473,13.3974667050661));
#15562=CARTESIAN_POINT('Ctrl Pts',(0.254082853280636,0.178297434879117,
13.3921693092328));
#15563=CARTESIAN_POINT('Ctrl Pts',(0.28218455619408,0.0849572034945515,
13.3868719133995));
#15564=CARTESIAN_POINT('Ctrl Pts',(0.310286259107524,-0.00838302789001326,
13.3815745175661));
#15565=CARTESIAN_POINT('Ctrl Pts',(0.287485350461608,-0.117047970666788,
13.3762771217328));
#15566=CARTESIAN_POINT('Ctrl Pts',(0.224234622987472,-0.191219290305052,
13.3709797258995));
#15567=CARTESIAN_POINT('Ctrl Pts',(0.160983895513336,-0.265390609943316,
13.3656823300661));
#15568=CARTESIAN_POINT('Ctrl Pts',(0.0572833492109803,-0.305068306443069,
13.3603849342328));
#15569=CARTESIAN_POINT('Ctrl Pts',(-0.0393235254694371,-0.292061093472824,
13.3550875383995));
#15570=CARTESIAN_POINT('Ctrl Pts',(-0.135930400149854,-0.279053880502579,
13.3497901425661));
#15571=CARTESIAN_POINT('Ctrl Pts',(-0.225443603208334,-0.213361758062335,
13.3444927467328));
#15572=CARTESIAN_POINT('Ctrl Pts',(-0.266824525222594,-0.125102530702081,
13.3391953508995));
#15573=CARTESIAN_POINT('Ctrl Pts',(-0.284993533188177,-0.0863507937448422,
13.336869437836));
#15574=CARTESIAN_POINT('Ctrl Pts',(-0.293883597264882,-0.0432485690121582,
13.3345435247725));
#15575=CARTESIAN_POINT('Ctrl Pts',(-0.293756705318437,-9.65891231691218E-5,
13.332217611709));
#15576=CARTESIAN_POINT('Ctrl Pts',(-0.293733177601347,-5.56197620117739E-5,
13.317782388291));
#15577=CARTESIAN_POINT('Ctrl Pts',(-0.293810260893271,-0.0458992684706001,
13.3202529066628));
#15578=CARTESIAN_POINT('Ctrl Pts',(-0.28373102046765,-0.0917108359027396,
13.3227234250346));
#15579=CARTESIAN_POINT('Ctrl Pts',(-0.263318357641365,-0.132329391391207,
13.3251939434064));
#15580=CARTESIAN_POINT('Ctrl Pts',(-0.219485873061089,-0.219550359193053,
13.3304989327337));
#15581=CARTESIAN_POINT('Ctrl Pts',(-0.12800622670986,-0.282826474015431,
13.335803922061));
#15582=CARTESIAN_POINT('Ctrl Pts',(-0.0309298619793288,-0.29307161036645,
13.3411089113884));
#15583=CARTESIAN_POINT('Ctrl Pts',(0.0661465027512023,-0.303316746717469,
13.3464139007157));
#15584=CARTESIAN_POINT('Ctrl Pts',(0.168819585861035,-0.260530904597129,
13.351718890043));
#15585=CARTESIAN_POINT('Ctrl Pts',(0.229893678370732,-0.184381450923717,
13.3570238793704));
#15586=CARTESIAN_POINT('Ctrl Pts',(0.290967770880429,-0.108231997250306,
13.3623288686977));
#15587=CARTESIAN_POINT('Ctrl Pts',(0.31044287278999,0.00128106797617772,
13.3676338580251));
#15588=CARTESIAN_POINT('Ctrl Pts',(0.27936683882728,0.0938178980565548,
13.3729388473524));
#15589=CARTESIAN_POINT('Ctrl Pts',(0.24829080486457,0.186354728136933,13.3782438366797));
#15590=CARTESIAN_POINT('Ctrl Pts',(0.166663635029587,0.261915323071205,
13.3835488260071));
#15591=CARTESIAN_POINT('Ctrl Pts',(0.0720069368793092,0.285766734827215,
13.3888538153344));
#15592=CARTESIAN_POINT('Ctrl Pts',(-0.0226497612709665,0.309618146583224,
13.3941588046617));
#15593=CARTESIAN_POINT('Ctrl Pts',(-0.130335987736536,0.281760375160974,
13.3994637939891));
#15594=CARTESIAN_POINT('Ctrl Pts',(-0.201551747218579,0.214998838681592,
13.4047687833164));
#15595=CARTESIAN_POINT('Ctrl Pts',(-0.259784585821543,0.160408200219468,
13.4091066516413));
#15596=CARTESIAN_POINT('Ctrl Pts',(-0.293632297236924,0.0798054665620052,
13.4134445199662));
#15597=CARTESIAN_POINT('Ctrl Pts',(-0.294362671296069,-0.000253937998619662,
13.417782388291));
#15598=CARTESIAN_POINT('Origin',(0.,0.,12.6151410108095));
#15599=CARTESIAN_POINT('',(-0.237384871732189,-0.000177998745596757,13.4651410108095));
#15600=CARTESIAN_POINT('',(-0.237480735682898,0.000138191412729517,13.4848589891905));
#15601=CARTESIAN_POINT('',(-0.237175,-1.00305832390001E-14,12.6151410108095));
#15602=CARTESIAN_POINT('',(-0.234668236863855,0.0343918483395353,13.562825));
#15603=CARTESIAN_POINT('Ctrl Pts',(-0.237384871732189,-0.000177998745596738,
13.4651410108095));
#15604=CARTESIAN_POINT('Ctrl Pts',(-0.237482278815476,-0.0117279779843829,
13.4659179655397));
#15605=CARTESIAN_POINT('Ctrl Pts',(-0.23146378830816,-0.101926256035546,
13.4719923161032));
#15606=CARTESIAN_POINT('Ctrl Pts',(-0.115844693426342,-0.255404084499389,
13.4833640625));
#15607=CARTESIAN_POINT('Ctrl Pts',(0.151994963678255,-0.235653121630174,
13.49925625));
#15608=CARTESIAN_POINT('Ctrl Pts',(0.280386067331958,7.16919272130007E-5,
13.5151484375));
#15609=CARTESIAN_POINT('Ctrl Pts',(0.151848011613721,0.23594581398157,13.531040625));
#15610=CARTESIAN_POINT('Ctrl Pts',(-0.116259094268414,0.255025114686607,
13.5469328125));
#15611=CARTESIAN_POINT('Ctrl Pts',(-0.223221075339677,0.112500043789072,
13.5575276041667));
#15612=CARTESIAN_POINT('Ctrl Pts',(-0.234668236863856,0.0343918483395283,
13.562825));
#15613=CARTESIAN_POINT('',(-0.0439445221993903,0.233068358199193,13.562825));
#15614=CARTESIAN_POINT('Origin',(0.,0.,13.562825));
#15615=CARTESIAN_POINT('Ctrl Pts',(-0.237480735682898,0.000138191412729494,
13.4848589891905));
#15616=CARTESIAN_POINT('Ctrl Pts',(-0.236987434834035,-0.0706816697969668,
13.489627702151));
#15617=CARTESIAN_POINT('Ctrl Pts',(-0.165686680756775,-0.221141686642749,
13.4997014044388));
#15618=CARTESIAN_POINT('Ctrl Pts',(0.0903269506402298,-0.265580501456578,
13.515080096054));
#15619=CARTESIAN_POINT('Ctrl Pts',(0.272486967933624,-0.0674994743880085,
13.530995064036));
#15620=CARTESIAN_POINT('Ctrl Pts',(0.203600577200948,0.19281335099551,13.546910032018));
#15621=CARTESIAN_POINT('Ctrl Pts',(0.0337423613347716,0.2477160478489,13.5575200106727));
#15622=CARTESIAN_POINT('Ctrl Pts',(-0.043944522199392,0.233068358199193,
13.562825));
#15623=CARTESIAN_POINT('Origin',(0.,0.,12.6151410108095));
#15624=CARTESIAN_POINT('',(-0.236817629449015,-7.78671831719857E-5,13.3651410108095));
#15625=CARTESIAN_POINT('',(-0.237306140600426,-0.000204717011637295,13.3848589891905));
#15626=CARTESIAN_POINT('',(-0.237175,-1.00305832390001E-14,12.6151410108095));
#15627=CARTESIAN_POINT('Ctrl Pts',(-0.236817629449016,-7.78671831719799E-5,
13.3651410108095));
#15628=CARTESIAN_POINT('Ctrl Pts',(-0.236919925837179,-0.0348656674216854,
13.367466923873));
#15629=CARTESIAN_POINT('Ctrl Pts',(-0.213430025619855,-0.148753143302577,
13.3750902327698));
#15630=CARTESIAN_POINT('Ctrl Pts',(-0.0374201180154527,-0.277923634425439,
13.3880109375));
#15631=CARTESIAN_POINT('Ctrl Pts',(0.213380463928066,-0.18196281524805,
13.403903125));
#15632=CARTESIAN_POINT('Ctrl Pts',(0.268524639741408,0.0808441983795663,
13.4197953125));
#15633=CARTESIAN_POINT('Ctrl Pts',(0.077452087548127,0.269525343391667,
13.4356875));
#15634=CARTESIAN_POINT('Ctrl Pts',(-0.171829534519279,0.213922458814076,
13.4508027327698));
#15635=CARTESIAN_POINT('Ctrl Pts',(-0.236818142467366,0.0670215417996536,
13.4606205697063));
#15636=CARTESIAN_POINT('Ctrl Pts',(-0.237384871732189,-0.000177998745596738,
13.4651410108095));
#15637=CARTESIAN_POINT('Ctrl Pts',(-0.237306140600426,-0.000204717011637273,
13.3848589891905));
#15638=CARTESIAN_POINT('Ctrl Pts',(-0.23743741378788,-0.0145941289722833,
13.385826110193));
#15639=CARTESIAN_POINT('Ctrl Pts',(-0.229682327632944,-0.107773186042249,
13.3920982205228));
#15640=CARTESIAN_POINT('Ctrl Pts',(-0.106286584194727,-0.259655320928406,
13.4036753201799));
#15641=CARTESIAN_POINT('Ctrl Pts',(0.161056632784338,-0.229734753162831,
13.4195902881619));
#15642=CARTESIAN_POINT('Ctrl Pts',(0.280337460803119,0.0113889577443968,
13.4355052561439));
#15643=CARTESIAN_POINT('Ctrl Pts',(0.141885966824002,0.242044705653255,
13.4514202241259));
#15644=CARTESIAN_POINT('Ctrl Pts',(-0.126992591218768,0.250174275017661,
13.4673351921079));
#15645=CARTESIAN_POINT('Ctrl Pts',(-0.233558987596684,0.0947948497711226,
13.4784814471295));
#15646=CARTESIAN_POINT('Ctrl Pts',(-0.237536210941985,0.00810239856573657,
13.4843227128237));
#15647=CARTESIAN_POINT('Ctrl Pts',(-0.237480735682898,0.000138191412729494,
13.4848589891905));
#15648=CARTESIAN_POINT('Origin',(0.,0.,12.6151410108095));
#15649=CARTESIAN_POINT('',(-0.237100373739744,0.000214889078547364,13.2651410108095));
#15650=CARTESIAN_POINT('',(-0.236798662126443,-4.48389431123158E-5,13.2848589891905));
#15651=CARTESIAN_POINT('',(-0.237175,-1.00305832390001E-14,12.6151410108095));
#15652=CARTESIAN_POINT('Ctrl Pts',(-0.237100373739744,0.000214889078547369,
13.2651410108095));
#15653=CARTESIAN_POINT('Ctrl Pts',(-0.23659111649862,-0.0575662489871676,
13.2690158822063));
#15654=CARTESIAN_POINT('Ctrl Pts',(-0.18624470561426,-0.195135369386986,
13.2781881494365));
#15655=CARTESIAN_POINT('Ctrl Pts',(0.0441614921479,-0.276932241019365,13.2926578125));
#15656=CARTESIAN_POINT('Ctrl Pts',(0.256726031781252,-0.1128425796642,13.30855));
#15657=CARTESIAN_POINT('Ctrl Pts',(0.233890236562906,0.154716040176168,
13.3244421875));
#15658=CARTESIAN_POINT('Ctrl Pts',(-0.00340698100913133,0.280410602722076,
13.340334375));
#15659=CARTESIAN_POINT('Ctrl Pts',(-0.20330767467579,0.168222136646133,
13.3539006494365));
#15660=CARTESIAN_POINT('Ctrl Pts',(-0.236686940146988,0.0443654745011182,
13.3621695280397));
#15661=CARTESIAN_POINT('Ctrl Pts',(-0.236817629449016,-7.78671831719799E-5,
13.3651410108095));
#15662=CARTESIAN_POINT('Ctrl Pts',(-0.236798662126443,-4.48389431123193E-5,
13.2848589891905));
#15663=CARTESIAN_POINT('Ctrl Pts',(-0.236860804307819,-0.0370025798760042,
13.2873295075623));
#15664=CARTESIAN_POINT('Ctrl Pts',(-0.211287036747699,-0.153238955594931,
13.2951050152614));
#15665=CARTESIAN_POINT('Ctrl Pts',(-0.0294466067184147,-0.279017272289624,
13.3081855122878));
#15666=CARTESIAN_POINT('Ctrl Pts',(0.218869047461476,-0.175539378629952,
13.3241004802698));
#15667=CARTESIAN_POINT('Ctrl Pts',(0.265969733682413,0.0893188257727471,
13.3400154482518));
#15668=CARTESIAN_POINT('Ctrl Pts',(0.0685537852907199,0.272062715339731,
13.3559304162339));
#15669=CARTESIAN_POINT('Ctrl Pts',(-0.176059774813894,0.208782676027031,
13.3708782632134));
#15670=CARTESIAN_POINT('Ctrl Pts',(-0.236717335476437,0.0643367149280847,
13.3805211208656));
#15671=CARTESIAN_POINT('Ctrl Pts',(-0.237306140600426,-0.000204717011637273,
13.3848589891905));
#15672=CARTESIAN_POINT('Origin',(0.,0.,12.6151410108095));
#15673=CARTESIAN_POINT('',(-0.237568867267691,-3.50085230488751E-5,13.1651410108095));
#15674=CARTESIAN_POINT('',(-0.23714100096821,0.000219260706363564,13.1848589891905));
#15675=CARTESIAN_POINT('',(-0.237175,-1.00305832390001E-14,12.6151410108095));
#15676=CARTESIAN_POINT('Ctrl Pts',(-0.237568867267691,-3.50085230488705E-5,
13.1651410108095));
#15677=CARTESIAN_POINT('Ctrl Pts',(-0.23757272817366,-0.00191072693511385,
13.1652674447063));
#15678=CARTESIAN_POINT('Ctrl Pts',(-0.236702342150314,-0.0823726342805651,
13.1706912744365));
#15679=CARTESIAN_POINT('Ctrl Pts',(-0.14620196384549,-0.239304592799359,
13.1814125));
#15680=CARTESIAN_POINT('Ctrl Pts',(0.12200497990914,-0.252500469855226,
13.1973046875));
#15681=CARTESIAN_POINT('Ctrl Pts',(0.278341649769444,-0.034170578184477,
13.213196875));
#15682=CARTESIAN_POINT('Ctrl Pts',(0.179457945287098,0.215491410897154,
13.2290890625));
#15683=CARTESIAN_POINT('Ctrl Pts',(-0.0839764970484053,0.267562423440159,
13.24498125));
#15684=CARTESIAN_POINT('Ctrl Pts',(-0.224953486042581,0.121419348905117,
13.2569985661032));
#15685=CARTESIAN_POINT('Ctrl Pts',(-0.237287329846353,0.0214272268439697,
13.263718486373));
#15686=CARTESIAN_POINT('Ctrl Pts',(-0.237100373739744,0.000214889078547369,
13.2651410108095));
#15687=CARTESIAN_POINT('Ctrl Pts',(-0.23714100096821,0.000219260706363571,
13.1848589891905));
#15688=CARTESIAN_POINT('Ctrl Pts',(-0.236601917095457,-0.0590126279016519,
13.1888329049316));
#15689=CARTESIAN_POINT('Ctrl Pts',(-0.184121441521327,-0.198168150201175,
13.19811181));
#15690=CARTESIAN_POINT('Ctrl Pts',(0.0497427765240963,-0.276122067797826,
13.2126957043958));
#15691=CARTESIAN_POINT('Ctrl Pts',(0.259221295320457,-0.107340859314887,
13.2286106723778));
#15692=CARTESIAN_POINT('Ctrl Pts',(0.23038737805747,0.160123065998856,13.2445256403598));
#15693=CARTESIAN_POINT('Ctrl Pts',(-0.0102508111899536,0.280379494845555,
13.2604406083418));
#15694=CARTESIAN_POINT('Ctrl Pts',(-0.205573087853117,0.164217542086628,
13.273885057952));
#15695=CARTESIAN_POINT('Ctrl Pts',(-0.236727365264118,0.0423574538123621,
13.2820245182349));
#15696=CARTESIAN_POINT('Ctrl Pts',(-0.236798662126443,-4.48389431123193E-5,
13.2848589891905));
#15697=CARTESIAN_POINT('Origin',(0.,0.,12.6151410108095));
#15698=CARTESIAN_POINT('',(-0.236996339228359,-0.000195082766924492,13.0651410108095));
#15699=CARTESIAN_POINT('',(-0.237565807314834,-4.77927823669955E-5,13.0848589891905));
#15700=CARTESIAN_POINT('',(-0.237175,-1.00305832390001E-14,12.6151410108095));
#15701=CARTESIAN_POINT('Ctrl Pts',(-0.236996339228359,-0.000195082766924502,
13.0651410108095));
#15702=CARTESIAN_POINT('Ctrl Pts',(-0.237189817656082,-0.0252059024681657,
13.0668164030397));
#15703=CARTESIAN_POINT('Ctrl Pts',(-0.222022384094442,-0.129069373509938,
13.0737891911032));
#15704=CARTESIAN_POINT('Ctrl Pts',(-0.0711327326516408,-0.271259720491414,
13.086059375));
#15705=CARTESIAN_POINT('Ctrl Pts',(0.189521520535091,-0.206696143611909,
13.1019515625));
#15706=CARTESIAN_POINT('Ctrl Pts',(0.276397422085156,0.0473937502037132,
13.11784375));
#15707=CARTESIAN_POINT('Ctrl Pts',(0.109835673593312,0.258026795320596,
13.1337359375));
#15708=CARTESIAN_POINT('Ctrl Pts',(-0.155311566263621,0.232273338104525,
13.1495016911032));
#15709=CARTESIAN_POINT('Ctrl Pts',(-0.237410961845922,0.0766791381988347,
13.159970048873));
#15710=CARTESIAN_POINT('Ctrl Pts',(-0.237568867267691,-3.50085230488705E-5,
13.1651410108095));
#15711=CARTESIAN_POINT('Ctrl Pts',(-0.237565807314834,-4.77927823669981E-5,
13.0848589891905));
#15712=CARTESIAN_POINT('Ctrl Pts',(-0.237572826099328,-0.0026043933601553,
13.0850313129736));
#15713=CARTESIAN_POINT('Ctrl Pts',(-0.236375116521228,-0.0838592301393141,
13.090508626084));
#15714=CARTESIAN_POINT('Ctrl Pts',(-0.143851548471854,-0.240882693501056,
13.1012909285217));
#15715=CARTESIAN_POINT('Ctrl Pts',(0.124964166840451,-0.25120051183695,
13.1172058965037));
#15716=CARTESIAN_POINT('Ctrl Pts',(0.278895358440525,-0.030579718254803,
13.1331208644857));
#15717=CARTESIAN_POINT('Ctrl Pts',(0.176426965387693,0.218154225247527,
13.1490358324677));
#15718=CARTESIAN_POINT('Ctrl Pts',(-0.0882377470317194,0.266330321450576,
13.1649508004497));
#15719=CARTESIAN_POINT('Ctrl Pts',(-0.225951591446148,0.118766717192262,
13.1768918526907));
#15720=CARTESIAN_POINT('Ctrl Pts',(-0.237321568536963,0.0200591384307359,
13.1835279156042));
#15721=CARTESIAN_POINT('Ctrl Pts',(-0.23714100096821,0.000219260706363571,
13.1848589891905));
#15722=CARTESIAN_POINT('Origin',(0.,0.,12.6151410108095));
#15723=CARTESIAN_POINT('',(-0.236868258229183,0.000132495174343476,12.9651410108095));
#15724=CARTESIAN_POINT('',(-0.236995674286161,-0.00019678875968307,12.9848589891905));
#15725=CARTESIAN_POINT('',(-0.237175,-1.00305832390001E-14,12.6151410108095));
#15726=CARTESIAN_POINT('Ctrl Pts',(-0.236868258229183,0.000132495174343491,
12.9651410108095));
#15727=CARTESIAN_POINT('Ctrl Pts',(-0.23662421943674,-0.0480671567343035,
12.968365361373));
#15728=CARTESIAN_POINT('Ctrl Pts',(-0.198883081137399,-0.175806934565607,
12.9768871077698));
#15729=CARTESIAN_POINT('Ctrl Pts',(0.00995747728231949,-0.28025434325381,
12.99070625));
#15730=CARTESIAN_POINT('Ctrl Pts',(0.240996248429915,-0.143396350591946,
13.0065984375));
#15731=CARTESIAN_POINT('Ctrl Pts',(0.251057922280563,0.124946521755194,
13.022490625));
#15732=CARTESIAN_POINT('Ctrl Pts',(0.0309165058329335,0.27872184254975,
13.0383828125));
#15733=CARTESIAN_POINT('Ctrl Pts',(-0.191376846905649,0.187659544819706,
13.0525996077698));
#15734=CARTESIAN_POINT('Ctrl Pts',(-0.236578061317235,0.0538754073814997,
13.0615190072063));
#15735=CARTESIAN_POINT('Ctrl Pts',(-0.236996339228359,-0.000195082766924502,
13.0651410108095));
#15736=CARTESIAN_POINT('Ctrl Pts',(-0.236995674286161,-0.000196788759683073,
12.9848589891905));
#15737=CARTESIAN_POINT('Ctrl Pts',(-0.237190390924988,-0.025212537514768,
12.9865347103429));
#15738=CARTESIAN_POINT('Ctrl Pts',(-0.222007629560777,-0.129192695194398,
12.9935154208226));
#15739=CARTESIAN_POINT('Ctrl Pts',(-0.0707617483345123,-0.271496792539298,
13.0058011206296));
#15740=CARTESIAN_POINT('Ctrl Pts',(0.19021711870995,-0.20624060859311,13.0217160886116));
#15741=CARTESIAN_POINT('Ctrl Pts',(0.276321843237659,0.0486207800379639,
13.0376310565936));
#15742=CARTESIAN_POINT('Ctrl Pts',(0.108392911780422,0.258783144727794,
13.0535460245757));
#15743=CARTESIAN_POINT('Ctrl Pts',(-0.156288642347958,0.231336327613849,
13.0692886687746));
#15744=CARTESIAN_POINT('Ctrl Pts',(-0.237356752750831,0.0761005801423566,
13.0797263236462));
#15745=CARTESIAN_POINT('Ctrl Pts',(-0.237565807314834,-4.77927823669981E-5,
13.0848589891905));
#15746=CARTESIAN_POINT('Origin',(0.,0.,12.6151410108095));
#15747=CARTESIAN_POINT('',(-0.237475867347687,0.000143668378376509,12.8651410108095));
#15748=CARTESIAN_POINT('',(-0.23685325391662,0.000124198907147655,12.8848589891905));
#15749=CARTESIAN_POINT('',(-0.237175,-1.00305832390001E-14,12.6151410108095));
#15750=CARTESIAN_POINT('Ctrl Pts',(-0.237475867347687,0.000143668378376506,
12.8651410108095));
#15751=CARTESIAN_POINT('Ctrl Pts',(-0.236995427452231,-0.0707374005589641,
12.8699143197063));
#15752=CARTESIAN_POINT('Ctrl Pts',(-0.165656267828233,-0.221154079023818,
12.8799850244365));
#15753=CARTESIAN_POINT('Ctrl Pts',(0.0902083908256771,-0.26551977706768,
12.895353125));
#15754=CARTESIAN_POINT('Ctrl Pts',(0.27207046341544,-0.0679625719645133,
12.9112453125));
#15755=CARTESIAN_POINT('Ctrl Pts',(0.204468796870817,0.191925109618724,
12.9271375));
#15756=CARTESIAN_POINT('Ctrl Pts',(-0.0506199491430696,0.275824015104995,
12.9430296875));
#15757=CARTESIAN_POINT('Ctrl Pts',(-0.216954845886699,0.141104430820563,
12.9556975244365));
#15758=CARTESIAN_POINT('Ctrl Pts',(-0.237025159116467,0.0311217001100208,
12.9630679655397));
#15759=CARTESIAN_POINT('Ctrl Pts',(-0.236868258229183,0.000132495174343491,
12.9651410108095));
#15760=CARTESIAN_POINT('Ctrl Pts',(-0.23685325391662,0.000124198907147644,
12.8848589891905));
#15761=CARTESIAN_POINT('Ctrl Pts',(-0.236630679274289,-0.0474065074335064,
12.8880381077122));
#15762=CARTESIAN_POINT('Ctrl Pts',(-0.199669376887335,-0.174571568479624,
12.8965222155612));
#15763=CARTESIAN_POINT('Ctrl Pts',(0.00797328488061451,-0.280452709922419,
12.9103113127376));
#15764=CARTESIAN_POINT('Ctrl Pts',(0.240296121102423,-0.14482920233622,
12.9262262807196));
#15765=CARTESIAN_POINT('Ctrl Pts',(0.251706166281744,0.123942967091746,
12.9421412487016));
#15766=CARTESIAN_POINT('Ctrl Pts',(0.0317122558575804,0.278768752799521,
12.9580562166836));
#15767=CARTESIAN_POINT('Ctrl Pts',(-0.191202431084563,0.187994314674536,
12.9722954635132));
#15768=CARTESIAN_POINT('Ctrl Pts',(-0.236573958000352,0.0539821900646985,
12.9812297210155));
#15769=CARTESIAN_POINT('Ctrl Pts',(-0.236995674286161,-0.000196788759683073,
12.9848589891905));
#15770=CARTESIAN_POINT('Origin',(0.,0.,13.55));
#15771=CARTESIAN_POINT('',(-0.286968182007205,0.000164849531348759,13.5133965297371));
#15772=CARTESIAN_POINT('Ctrl Pts',(-0.043944522199392,0.233068358199193,
13.562825));
#15773=CARTESIAN_POINT('Ctrl Pts',(-0.0294765840042651,0.236438793486496,
13.5621935878038));
#15774=CARTESIAN_POINT('Ctrl Pts',(-0.0147452085483875,0.238326827796529,
13.5615668352976));
#15775=CARTESIAN_POINT('Ctrl Pts',(6.08274638918418E-5,0.238832568630261,
13.560941941181));
#15776=CARTESIAN_POINT('Ctrl Pts',(0.00713427631766705,0.239074181707367,
13.5606434037083));
#15777=CARTESIAN_POINT('Ctrl Pts',(0.0142250285277132,0.2389995429081,13.5603452903877));
#15778=CARTESIAN_POINT('Ctrl Pts',(0.0213132083401427,0.238615554436029,
13.5600472957714));
#15779=CARTESIAN_POINT('Ctrl Pts',(0.0261835574655618,0.238351712664431,
13.5598425411155));
#15780=CARTESIAN_POINT('Ctrl Pts',(0.0310529721761364,0.237941454616689,
13.5596378302422));
#15781=CARTESIAN_POINT('Ctrl Pts',(0.0358999420287469,0.237388908068873,
13.5594336980816));
#15782=CARTESIAN_POINT('Ctrl Pts',(0.0493536867081515,0.235855203423731,
13.558867088003));
#15783=CARTESIAN_POINT('Ctrl Pts',(0.0626628489801356,0.23322660375155,
13.5583037466019));
#15784=CARTESIAN_POINT('Ctrl Pts',(0.0756903340245162,0.229556977452041,
13.5577416326332));
#15785=CARTESIAN_POINT('Ctrl Pts',(0.0818558888395591,0.227820242999976,
13.5574755993602));
#15786=CARTESIAN_POINT('Ctrl Pts',(0.087958354013132,0.225849872295259,
13.5572098410162));
#15787=CARTESIAN_POINT('Ctrl Pts',(0.0939827769363731,0.223649197682829,
13.5569441412149));
#15788=CARTESIAN_POINT('Ctrl Pts',(0.0979230858746843,0.222209833621548,
13.5567703587108));
#15789=CARTESIAN_POINT('Ctrl Pts',(0.101826955013135,0.220672876108273,
13.5565967330609));
#15790=CARTESIAN_POINT('Ctrl Pts',(0.105682387170434,0.219043149639582,
13.5564235627486));
#15791=CARTESIAN_POINT('Ctrl Pts',(0.119489970730244,0.21320655766286,13.5558033823229));
#15792=CARTESIAN_POINT('Ctrl Pts',(0.132707719562554,0.206172506490602,
13.5551876986953));
#15793=CARTESIAN_POINT('Ctrl Pts',(0.145152214688433,0.198000823300654,
13.5545738505959));
#15794=CARTESIAN_POINT('Ctrl Pts',(0.151794873917279,0.19363891820062,13.5542461889511));
#15795=CARTESIAN_POINT('Ctrl Pts',(0.158217051111106,0.188952135332664,
13.5539190502927));
#15796=CARTESIAN_POINT('Ctrl Pts',(0.164388452074525,0.183944806507876,
13.5535920298744));
#15797=CARTESIAN_POINT('Ctrl Pts',(0.168212225599151,0.180842287079498,
13.5533894094281));
#15798=CARTESIAN_POINT('Ctrl Pts',(0.171939685169454,0.17761664713226,13.553186834374));
#15799=CARTESIAN_POINT('Ctrl Pts',(0.175563092765558,0.174268326452765,
13.5529842084384));
#15800=CARTESIAN_POINT('Ctrl Pts',(0.177047466069561,0.172896645873624,
13.5529012002419));
#15801=CARTESIAN_POINT('Ctrl Pts',(0.178514082249302,0.171504603781964,
13.5528181987184));
#15802=CARTESIAN_POINT('Ctrl Pts',(0.179960409179589,0.170094285986212,
13.5527353145998));
#15803=CARTESIAN_POINT('Ctrl Pts',(0.190810527615469,0.159514302446048,
13.552113530905));
#15804=CARTESIAN_POINT('Ctrl Pts',(0.200553823179652,0.147879977988366,
13.5514965535525));
#15805=CARTESIAN_POINT('Ctrl Pts',(0.209172247663828,0.135414754877218,
13.5508817172788));
#15806=CARTESIAN_POINT('Ctrl Pts',(0.2150107423251,0.12697027193029,13.5504652005118));
#15807=CARTESIAN_POINT('Ctrl Pts',(0.220332398139305,0.118143361409001,
13.5500496663492));
#15808=CARTESIAN_POINT('Ctrl Pts',(0.225122317125784,0.108994362021549,
13.5496342861636));
#15809=CARTESIAN_POINT('Ctrl Pts',(0.227457000051293,0.104534993770087,
13.5494318232348));
#15810=CARTESIAN_POINT('Ctrl Pts',(0.229665233796247,0.0999990193216993,
13.5492293968869));
#15811=CARTESIAN_POINT('Ctrl Pts',(0.231744553284755,0.0953930457521194,
13.5490269111671));
#15812=CARTESIAN_POINT('Ctrl Pts',(0.233552950784709,0.0913872009869837,
13.5488508080375));
#15813=CARTESIAN_POINT('Ctrl Pts',(0.235260285198856,0.0873360923025083,
13.5486749987829));
#15814=CARTESIAN_POINT('Ctrl Pts',(0.236864416101865,0.083248529595993,
13.5484995890061));
#15815=CARTESIAN_POINT('Ctrl Pts',(0.242716576792444,0.0683363589330668,
13.547859662303));
#15816=CARTESIAN_POINT('Ctrl Pts',(0.247206036027669,0.0529249259443079,
13.5472243423549));
#15817=CARTESIAN_POINT('Ctrl Pts',(0.25028385037818,0.0372383602707011,
13.5465907037737));
#15818=CARTESIAN_POINT('Ctrl Pts',(0.252087300804334,0.0280467910832205,
13.5462194221955));
#15819=CARTESIAN_POINT('Ctrl Pts',(0.253405246706662,0.0187601746905643,
13.5458487178968));
#15820=CARTESIAN_POINT('Ctrl Pts',(0.254219891160352,0.00942114969984719,
13.5454780023471));
#15821=CARTESIAN_POINT('Ctrl Pts',(0.25478813976954,0.00290678881749256,
13.5452194127323));
#15822=CARTESIAN_POINT('Ctrl Pts',(0.255111030741479,-0.00363999231176376,
13.5449605458955));
#15823=CARTESIAN_POINT('Ctrl Pts',(0.255181476734096,-0.0101677045994756,
13.5447026610801));
#15824=CARTESIAN_POINT('Ctrl Pts',(0.255354370584029,-0.0261885067310612,
13.5440697407832));
#15825=CARTESIAN_POINT('Ctrl Pts',(0.254016166114596,-0.0421255321420965,
13.5434414744878));
#15826=CARTESIAN_POINT('Ctrl Pts',(0.251097893857644,-0.0577648854388578,
13.5428150415744));
#15827=CARTESIAN_POINT('Ctrl Pts',(0.250834755331568,-0.0591750747608081,
13.5427585565658));
#15828=CARTESIAN_POINT('Ctrl Pts',(0.250558734870263,-0.0605828459371271,
13.5427020864635));
#15829=CARTESIAN_POINT('Ctrl Pts',(0.250269760531176,-0.0619880420672277,
13.5426456291996));
#15830=CARTESIAN_POINT('Ctrl Pts',(0.248732768931078,-0.0694619743730475,
13.542345345304));
#15831=CARTESIAN_POINT('Ctrl Pts',(0.246829549128523,-0.0768631173570905,
13.5420454246012));
#15832=CARTESIAN_POINT('Ctrl Pts',(0.24457758894315,-0.0841750034805435,
13.5417455559504));
#15833=CARTESIAN_POINT('Ctrl Pts',(0.24320401817551,-0.0886348483306972,
13.5415626527109));
#15834=CARTESIAN_POINT('Ctrl Pts',(0.241700647647705,-0.0930614748590947,
13.5413797688365));
#15835=CARTESIAN_POINT('Ctrl Pts',(0.240070956053578,-0.0974509732874261,
13.5411968337233));
#15836=CARTESIAN_POINT('Ctrl Pts',(0.238427550824986,-0.101877408751667,
13.5410123592358));
#15837=CARTESIAN_POINT('Ctrl Pts',(0.236658304736593,-0.106258675580407,
13.5408281394574));
#15838=CARTESIAN_POINT('Ctrl Pts',(0.234770897270819,-0.110584625391991,
13.540644379461));
#15839=CARTESIAN_POINT('Ctrl Pts',(0.228360906593042,-0.125276364440202,
13.5400202959576));
#15840=CARTESIAN_POINT('Ctrl Pts',(0.220583153832133,-0.139355014290968,
13.5394005216076));
#15841=CARTESIAN_POINT('Ctrl Pts',(0.211608093803175,-0.15267492911545,
13.5387823454488));
#15842=CARTESIAN_POINT('Ctrl Pts',(0.205045157713066,-0.162415003213755,
13.5383303094057));
#15843=CARTESIAN_POINT('Ctrl Pts',(0.197840743027374,-0.171749337581638,
13.5378791279379));
#15844=CARTESIAN_POINT('Ctrl Pts',(0.190046593771134,-0.180613221027982,
13.5374277410453));
#15845=CARTESIAN_POINT('Ctrl Pts',(0.18689819700638,-0.184193730080112,
13.5372454061957));
#15846=CARTESIAN_POINT('Ctrl Pts',(0.183652322387751,-0.1876981824977,13.5370629859398));
#15847=CARTESIAN_POINT('Ctrl Pts',(0.180325161242096,-0.191109317049549,
13.5368811040816));
#15848=CARTESIAN_POINT('Ctrl Pts',(0.168744503055477,-0.202982256635035,
13.5362480383723));
#15849=CARTESIAN_POINT('Ctrl Pts',(0.156150610605738,-0.213764883234575,
13.5356196044284));
#15850=CARTESIAN_POINT('Ctrl Pts',(0.142703307452893,-0.223292717945068,
13.5349929842113));
#15851=CARTESIAN_POINT('Ctrl Pts',(0.13328997055946,-0.229962361439782,
13.5345543395892));
#15852=CARTESIAN_POINT('Ctrl Pts',(0.123457381914911,-0.236016716577223,
13.5341165837357));
#15853=CARTESIAN_POINT('Ctrl Pts',(0.113250289629505,-0.241387649069037,
13.5336787499942));
#15854=CARTESIAN_POINT('Ctrl Pts',(0.107437633034519,-0.244446246492947,
13.5334294157946));
#15855=CARTESIAN_POINT('Ctrl Pts',(0.101497232632265,-0.2472851876651,13.5331798094348));
#15856=CARTESIAN_POINT('Ctrl Pts',(0.0954700064811808,-0.249876992596412,
13.5329311101113));
#15857=CARTESIAN_POINT('Ctrl Pts',(0.0924351354571309,-0.251182036324465,
13.5328058832902));
#15858=CARTESIAN_POINT('Ctrl Pts',(0.0893771001161341,-0.252425149988217,
13.5326808351245));
#15859=CARTESIAN_POINT('Ctrl Pts',(0.0862971123270629,-0.253605021774803,
13.5325559437995));
#15860=CARTESIAN_POINT('Ctrl Pts',(0.071172071972524,-0.259399073442352,
13.5319426341176));
#15861=CARTESIAN_POINT('Ctrl Pts',(0.0555195588483159,-0.263672035534303,
13.5313331067171));
#15862=CARTESIAN_POINT('Ctrl Pts',(0.039552096653546,-0.266494984784699,
13.5307247782039));
#15863=CARTESIAN_POINT('Ctrl Pts',(0.028285188816394,-0.268486904893556,
13.5302955314514));
#15864=CARTESIAN_POINT('Ctrl Pts',(0.0168607381260563,-0.269755816583468,
13.5298668816188));
#15865=CARTESIAN_POINT('Ctrl Pts',(0.00534958536819863,-0.270312121070808,
13.5294379211004));
#15866=CARTESIAN_POINT('Ctrl Pts',(0.00115101094099197,-0.270515027403772,
13.5292814621688));
#15867=CARTESIAN_POINT('Ctrl Pts',(-0.00305507661402366,-0.270622704683305,
13.5291251120846));
#15868=CARTESIAN_POINT('Ctrl Pts',(-0.00725720002110199,-0.270636144905838,
13.5289691225271));
#15869=CARTESIAN_POINT('Ctrl Pts',(-0.0241769446018754,-0.270690261625018,
13.5283410344835));
#15870=CARTESIAN_POINT('Ctrl Pts',(-0.0410701020235392,-0.269222772099358,
13.5277173600727));
#15871=CARTESIAN_POINT('Ctrl Pts',(-0.057711020888307,-0.266291935802486,
13.5270953457536));
#15872=CARTESIAN_POINT('Ctrl Pts',(-0.0688902381852458,-0.264323026748199,
13.5266774822154));
#15873=CARTESIAN_POINT('Ctrl Pts',(-0.0799560150048115,-0.261692586303153,
13.5262603678815));
#15874=CARTESIAN_POINT('Ctrl Pts',(-0.0908391235420861,-0.258405107652052,
13.5258431679299));
#15875=CARTESIAN_POINT('Ctrl Pts',(-0.0950317449826877,-0.257138635537865,
13.5256824453334));
#15876=CARTESIAN_POINT('Ctrl Pts',(-0.0991994850387932,-0.25577373191658,
13.5255216219886));
#15877=CARTESIAN_POINT('Ctrl Pts',(-0.103330775485522,-0.254312914760898,
13.525360940178));
#15878=CARTESIAN_POINT('Ctrl Pts',(-0.119359411115515,-0.248645216928368,
13.5247375247519));
#15879=CARTESIAN_POINT('Ctrl Pts',(-0.134773006972199,-0.241563252903294,
13.5241188617021));
#15880=CARTESIAN_POINT('Ctrl Pts',(-0.149349294964951,-0.233107026334203,
13.5235022794556));
#15881=CARTESIAN_POINT('Ctrl Pts',(-0.157525060571445,-0.228363971972305,
13.5231564416176));
#15882=CARTESIAN_POINT('Ctrl Pts',(-0.165437317263121,-0.223187661340015,
13.5228112584068));
#15883=CARTESIAN_POINT('Ctrl Pts',(-0.17304417849703,-0.217578409204512,
13.5224662583993));
#15884=CARTESIAN_POINT('Ctrl Pts',(-0.17887039297022,-0.213282194909192,
13.5222020174758));
#15885=CARTESIAN_POINT('Ctrl Pts',(-0.184517406155673,-0.208731888546409,
13.5219378840244));
#15886=CARTESIAN_POINT('Ctrl Pts',(-0.189978938566547,-0.203943453156376,
13.521673646231));
#15887=CARTESIAN_POINT('Ctrl Pts',(-0.193403116199697,-0.200941282313685,
13.5215079789652));
#15888=CARTESIAN_POINT('Ctrl Pts',(-0.196754223511486,-0.197845265193714,
13.5213422693538));
#15889=CARTESIAN_POINT('Ctrl Pts',(-0.200020365596183,-0.194669931635478,
13.5211769999744));
#15890=CARTESIAN_POINT('Ctrl Pts',(-0.212036537758927,-0.182987845026729,
13.5205689721345));
#15891=CARTESIAN_POINT('Ctrl Pts',(-0.222942778207884,-0.170203637448647,
13.5199651042774));
#15892=CARTESIAN_POINT('Ctrl Pts',(-0.232682805209074,-0.156537147041984,
13.519362903645));
#15893=CARTESIAN_POINT('Ctrl Pts',(-0.241969469951098,-0.143506781254366,
13.5187887332263));
#15894=CARTESIAN_POINT('Ctrl Pts',(-0.250196294757052,-0.129672988479396,
13.5182160784383));
#15895=CARTESIAN_POINT('Ctrl Pts',(-0.257283810651443,-0.115198924292403,
13.5176427786581));
#15896=CARTESIAN_POINT('Ctrl Pts',(-0.259491932919989,-0.11068951592932,
13.5174641665704));
#15897=CARTESIAN_POINT('Ctrl Pts',(-0.261585787385611,-0.106124522483284,
13.5172857588748));
#15898=CARTESIAN_POINT('Ctrl Pts',(-0.263560449912049,-0.101516719136934,
13.5171077781986));
#15899=CARTESIAN_POINT('Ctrl Pts',(-0.270475851072545,-0.0853798814838883,
13.5164844778838));
#15900=CARTESIAN_POINT('Ctrl Pts',(-0.275946482637518,-0.0686925965880584,
13.5158653248676));
#15901=CARTESIAN_POINT('Ctrl Pts',(-0.279885783875338,-0.0516738313500138,
13.5152476263517));
#15902=CARTESIAN_POINT('Ctrl Pts',(-0.281958120038393,-0.0427208215332613,
13.5149226755812));
#15903=CARTESIAN_POINT('Ctrl Pts',(-0.283605922974178,-0.0336755953807322,
13.5145981273385));
#15904=CARTESIAN_POINT('Ctrl Pts',(-0.284810979317383,-0.0245681482391185,
13.5142735895868));
#15905=CARTESIAN_POINT('Ctrl Pts',(-0.285495319284535,-0.0193961161487672,
13.5140892877028));
#15906=CARTESIAN_POINT('Ctrl Pts',(-0.28603679820466,-0.014204004240413,
13.5139049892021));
#15907=CARTESIAN_POINT('Ctrl Pts',(-0.28643144246244,-0.00899727922140894,
13.5137206222854));
#15908=CARTESIAN_POINT('Ctrl Pts',(-0.286662860032101,-0.00594407972326887,
13.5136125103772));
#15909=CARTESIAN_POINT('Ctrl Pts',(-0.286843607970751,-0.00288741530408205,
13.5135044302464));
#15910=CARTESIAN_POINT('Ctrl Pts',(-0.28697292281753,0.000166992375313765,
13.5133965297371));
#15911=CARTESIAN_POINT('',(0.0261262957278421,0.292560460953161,13.5058));
#15912=CARTESIAN_POINT('Ctrl Pts',(0.0261206201035333,0.292499143797286,
13.5058));
#15913=CARTESIAN_POINT('Ctrl Pts',(0.00884643054260094,0.291825436047159,
13.5079854825731));
#15914=CARTESIAN_POINT('Ctrl Pts',(-0.00828334513464932,0.289706514159306,
13.5101847285682));
#15915=CARTESIAN_POINT('Ctrl Pts',(-0.0250574246257949,0.286137019621129,
13.5124084954842));
#15916=CARTESIAN_POINT('Ctrl Pts',(-0.0350258051457675,0.284015765823609,
13.5137300198526));
#15917=CARTESIAN_POINT('Ctrl Pts',(-0.0448683071666012,0.281381300825545,
13.5150602040358));
#15918=CARTESIAN_POINT('Ctrl Pts',(-0.0545358180860379,0.278224980453642,
13.5164013057481));
#15919=CARTESIAN_POINT('Ctrl Pts',(-0.0606603459790604,0.27622539934966,
13.5172509158404));
#15920=CARTESIAN_POINT('Ctrl Pts',(-0.0667145579989015,0.274016266063491,
13.5181049076087));
#15921=CARTESIAN_POINT('Ctrl Pts',(-0.072684837684636,0.27159431964496,
13.5189638550939));
#15922=CARTESIAN_POINT('Ctrl Pts',(-0.0764355024604301,0.270072798108449,
13.5195034653377));
#15923=CARTESIAN_POINT('Ctrl Pts',(-0.0801508179192932,0.268468026109448,
13.520044724687));
#15924=CARTESIAN_POINT('Ctrl Pts',(-0.0838198221478387,0.266783197590374,
13.5205866293988));
#15925=CARTESIAN_POINT('Ctrl Pts',(-0.0942230095561321,0.262005992184504,
13.5221231597279));
#15926=CARTESIAN_POINT('Ctrl Pts',(-0.104273334180971,0.256578412344035,
13.5236675754247));
#15927=CARTESIAN_POINT('Ctrl Pts',(-0.113901775440171,0.250492155939794,
13.5252236806533));
#15928=CARTESIAN_POINT('Ctrl Pts',(-0.126477796119793,0.242542698250774,
13.5272561603671));
#15929=CARTESIAN_POINT('Ctrl Pts',(-0.138335359995195,0.233469464109384,
13.5293085822151));
#15930=CARTESIAN_POINT('Ctrl Pts',(-0.149379447945921,0.223405603100387,
13.5313894227842));
#15931=CARTESIAN_POINT('Ctrl Pts',(-0.153219453627113,0.219906420223386,
13.5321129265848));
#15932=CARTESIAN_POINT('Ctrl Pts',(-0.156960833903308,0.216287355644465,
13.5328398660326));
#15933=CARTESIAN_POINT('Ctrl Pts',(-0.160598645982812,0.212553746141513,
13.5335705974367));
#15934=CARTESIAN_POINT('Ctrl Pts',(-0.163567294871897,0.209506921440021,
13.534166913278));
#15935=CARTESIAN_POINT('Ctrl Pts',(-0.166463512525863,0.2063871883392,13.5347650814277));
#15936=CARTESIAN_POINT('Ctrl Pts',(-0.169280235000242,0.203203670539578,
13.5353642364953));
#15937=CARTESIAN_POINT('Ctrl Pts',(-0.179529104895811,0.191620186531006,
13.5375443101058));
#15938=CARTESIAN_POINT('Ctrl Pts',(-0.188750918175532,0.179170970598589,
13.5397418585162));
#15939=CARTESIAN_POINT('Ctrl Pts',(-0.196842895670712,0.166013931025591,
13.5419679679277));
#15940=CARTESIAN_POINT('Ctrl Pts',(-0.203730824185022,0.154814598341739,
13.543862842512));
#15941=CARTESIAN_POINT('Ctrl Pts',(-0.209799618039609,0.143101506632859,
13.5457784109491));
#15942=CARTESIAN_POINT('Ctrl Pts',(-0.214959055570843,0.130969922145647,
13.5477215105393));
#15943=CARTESIAN_POINT('Ctrl Pts',(-0.216612406033525,0.127082335426442,
13.5483441800816));
#15944=CARTESIAN_POINT('Ctrl Pts',(-0.218171913124406,0.123151835124804,
13.5489696646219));
#15945=CARTESIAN_POINT('Ctrl Pts',(-0.219629934580908,0.11919478632138,
13.549596137626));
#15946=CARTESIAN_POINT('Ctrl Pts',(-0.224740451337889,0.105324918955647,
13.551791990623));
#15947=CARTESIAN_POINT('Ctrl Pts',(-0.228625673283085,0.0910885104257726,
13.5540064494166));
#15948=CARTESIAN_POINT('Ctrl Pts',(-0.231173355347657,0.0766269568750346,
13.5562511496559));
#15949=CARTESIAN_POINT('Ctrl Pts',(-0.233624712277369,0.0627121792016433,
13.5584109801792));
#15950=CARTESIAN_POINT('Ctrl Pts',(-0.234837706655883,0.0485878801050229,
13.5605988085852));
#15951=CARTESIAN_POINT('Ctrl Pts',(-0.234668236863856,0.0343918483395283,
13.562825));
#15952=CARTESIAN_POINT('',(-0.214330452128339,0.201110949933342,13.5058));
#15953=CARTESIAN_POINT('Origin',(0.,0.,13.5058));
#15954=CARTESIAN_POINT('Ctrl Pts',(-0.28697292281753,0.000166992375313765,
13.5133965297371));
#15955=CARTESIAN_POINT('Ctrl Pts',(-0.287381793203279,0.00982448242552759,
13.513055367651));
#15956=CARTESIAN_POINT('Ctrl Pts',(-0.287277908684719,0.0194726610186102,
13.512715528512));
#15957=CARTESIAN_POINT('Ctrl Pts',(-0.286645660444495,0.0290760529402092,
13.5123765729991));
#15958=CARTESIAN_POINT('Ctrl Pts',(-0.285612853120713,0.0447636466395815,
13.5118228731802));
#15959=CARTESIAN_POINT('Ctrl Pts',(-0.283172279973397,0.0603320811344235,
13.5112715312968));
#15960=CARTESIAN_POINT('Ctrl Pts',(-0.279438676347389,0.0756505557756192,
13.5107206323131));
#15961=CARTESIAN_POINT('Ctrl Pts',(-0.277817724983914,0.082301101694054,
13.510481458435));
#15962=CARTESIAN_POINT('Ctrl Pts',(-0.275952566041092,0.0889045063031122,
13.5102423680381));
#15963=CARTESIAN_POINT('Ctrl Pts',(-0.27385050370512,0.0954496671937427,
13.5100032044105));
#15964=CARTESIAN_POINT('Ctrl Pts',(-0.272052647080838,0.101047627188955,
13.5097986520026));
#15965=CARTESIAN_POINT('Ctrl Pts',(-0.270079941233438,0.106606043452002,
13.5095939285241));
#15966=CARTESIAN_POINT('Ctrl Pts',(-0.267946682411625,0.112093614932915,
13.5093898414744));
#15967=CARTESIAN_POINT('Ctrl Pts',(-0.261495892531522,0.128687555721275,
13.5087726999153));
#15968=CARTESIAN_POINT('Ctrl Pts',(-0.253568602001536,0.144679477818713,
13.5081597540965));
#15969=CARTESIAN_POINT('Ctrl Pts',(-0.244320225481875,0.159886712194555,
13.50754839969));
#15970=CARTESIAN_POINT('Ctrl Pts',(-0.235493300050023,0.174400948674316,
13.5069649048737));
#15971=CARTESIAN_POINT('Ctrl Pts',(-0.225461890301029,0.188201490936452,
13.5063828597325));
#15972=CARTESIAN_POINT('Ctrl Pts',(-0.214321504642966,0.201109806014094,
13.5058));
#15973=CARTESIAN_POINT('',(-0.199999999999999,-2.4492935982947E-17,13.6));
#15974=CARTESIAN_POINT('',(-0.25,-3.06161699786838E-17,13.55));
#15975=CARTESIAN_POINT('Origin',(0.,0.,13.6));
#15976=CARTESIAN_POINT('Ctrl Pts',(0.170810875200406,-0.23953556085323,
12.7670766008995));
#15977=CARTESIAN_POINT('Ctrl Pts',(0.250539136060416,-0.182681981504947,
12.7723739967328));
#15978=CARTESIAN_POINT('Ctrl Pts',(0.347291359551364,0.0160604774249761,
12.7829687883995));
#15979=CARTESIAN_POINT('Ctrl Pts',(0.174450423592672,0.301171722453608,
12.7988609758995));
#15980=CARTESIAN_POINT('Ctrl Pts',(-0.158655251249622,0.309505572481922,
12.8147531633995));
#15981=CARTESIAN_POINT('Ctrl Pts',(-0.346141364686362,0.0343485950558648,
12.8306453508995));
#15982=CARTESIAN_POINT('Ctrl Pts',(-0.216309200137717,-0.272450359979308,
12.8465375383995));
#15983=CARTESIAN_POINT('Ctrl Pts',(0.111897580187261,-0.329359833090805,
12.8624297258995));
#15984=CARTESIAN_POINT('Ctrl Pts',(0.337485528984177,-0.0843031039188804,
12.8783219133995));
#15985=CARTESIAN_POINT('Ctrl Pts',(0.253630104519426,0.238070484873314,
12.8942141008995));
#15986=CARTESIAN_POINT('Ctrl Pts',(-0.0627907200922966,0.342141563165973,
12.9101062883995));
#15987=CARTESIAN_POINT('Ctrl Pts',(-0.321634866420445,0.132495983852973,
12.9259984758995));
#15988=CARTESIAN_POINT('Ctrl Pts',(-0.285562599947175,-0.198641295410301,
12.9418906633995));
#15989=CARTESIAN_POINT('Ctrl Pts',(0.0123515961482354,-0.347637094066705,
12.9577828508995));
#15990=CARTESIAN_POINT('Ctrl Pts',(0.298940007539078,-0.177873748684098,
12.9736750383995));
#15991=CARTESIAN_POINT('Ctrl Pts',(0.311420852682373,0.15498794856278,12.9895672258995));
#15992=CARTESIAN_POINT('Ctrl Pts',(0.0383498936061967,0.345736127661585,
13.0054594133994));
#15993=CARTESIAN_POINT('Ctrl Pts',(-0.269885287401924,0.219467827336637,
13.0213516008995));
#15994=CARTESIAN_POINT('Ctrl Pts',(-0.330654015328618,-0.108037577904655,
13.0372437883995));
#15995=CARTESIAN_POINT('Ctrl Pts',(-0.0882354799035033,-0.336479855670175,
13.0531359758995));
#15996=CARTESIAN_POINT('Ctrl Pts',(0.235088990582579,-0.256392981767151,
13.0690281633995));
#15997=CARTESIAN_POINT('Ctrl Pts',(0.342852836839687,0.0587888323387024,
13.0849203508995));
#15998=CARTESIAN_POINT('Ctrl Pts',(0.136243934525784,0.320065281683648,
13.1008125383995));
#15999=CARTESIAN_POINT('Ctrl Pts',(-0.195291395037498,0.287863622974583,
13.1167047258995));
#16000=CARTESIAN_POINT('Ctrl Pts',(-0.347757789320859,-0.00828941245669413,
13.1325969133995));
#16001=CARTESIAN_POINT('Ctrl Pts',(-0.18135392753597,-0.296841619907541,
13.1484891008995));
#16002=CARTESIAN_POINT('Ctrl Pts',(0.151339159225333,-0.313210238142333,
13.1643812883995));
#16003=CARTESIAN_POINT('Ctrl Pts',(0.34526452350446,-0.0423863564957258,
13.1802734758995));
#16004=CARTESIAN_POINT('Ctrl Pts',(0.222605786880847,0.267302932796215,
13.1961656633995));
#16005=CARTESIAN_POINT('Ctrl Pts',(-0.104167325526047,0.331893601670054,
13.2120578508995));
#16006=CARTESIAN_POINT('Ctrl Pts',(-0.335426081500374,0.0921603951917061,
13.2279500383995));
#16007=CARTESIAN_POINT('Ctrl Pts',(-0.259121917540537,-0.232077627176206,
13.2438422258995));
#16008=CARTESIAN_POINT('Ctrl Pts',(0.0547794286493582,-0.343516244578465,
13.2597344133995));
#16009=CARTESIAN_POINT('Ctrl Pts',(0.31845177000124,-0.139973803888303,
13.2756266008995));
#16010=CARTESIAN_POINT('Ctrl Pts',(0.290125466835911,0.191915079666188,
13.2915187883995));
#16011=CARTESIAN_POINT('Ctrl Pts',(-0.00422613602987575,0.34783092366748,
13.3074109758995));
#16012=CARTESIAN_POINT('Ctrl Pts',(-0.294702729176935,0.1848093612187,13.3233031633995));
#16013=CARTESIAN_POINT('Ctrl Pts',(-0.314956806266814,-0.147669635622091,
13.3391953508995));
#16014=CARTESIAN_POINT('Ctrl Pts',(-0.0464171970913749,-0.344746002942823,
13.3550875383995));
#16015=CARTESIAN_POINT('Ctrl Pts',(0.264684441815691,-0.225712913443562,
13.3709797258995));
#16016=CARTESIAN_POINT('Ctrl Pts',(0.333087167753441,0.100281914886762,
13.3868719133995));
#16017=CARTESIAN_POINT('Ctrl Pts',(0.0960742243350252,0.334328474863828,
13.4027641008994));
#16018=CARTESIAN_POINT('Ctrl Pts',(-0.229037672424893,0.261811459287546,
13.4186562883995));
#16019=CARTESIAN_POINT('Ctrl Pts',(-0.344126396035303,-0.0507542279728567,
13.4345484758994));
#16020=CARTESIAN_POINT('Ctrl Pts',(-0.143697728706779,-0.316811981278465,
13.4504406633995));
#16021=CARTESIAN_POINT('Ctrl Pts',(0.188539763103792,-0.292312209902382,
13.4663328508995));
#16022=CARTESIAN_POINT('Ctrl Pts',(0.347800489128543,8.89291240029669E-5,
13.4822250383995));
#16023=CARTESIAN_POINT('Ctrl Pts',(0.188357478725655,0.292675275528102,
13.4981172258995));
#16024=CARTESIAN_POINT('Ctrl Pts',(-0.144211765716315,0.316341894132181,
13.5140094133995));
#16025=CARTESIAN_POINT('Ctrl Pts',(-0.276891073531918,0.139548910647182,
13.5246042050661));
#16026=CARTESIAN_POINT('Ctrl Pts',(-0.291090525077881,0.0426608275808572,
13.5299016008995));
#16027=CARTESIAN_POINT('Ctrl Pts',(0.159774743137974,-0.224059110187407,
12.7780510672663));
#16028=CARTESIAN_POINT('Ctrl Pts',(0.23435174173247,-0.170878854385844,
12.7833484630996));
#16029=CARTESIAN_POINT('Ctrl Pts',(0.324852780604597,0.0150228060844386,
12.7939432547663));
#16030=CARTESIAN_POINT('Ctrl Pts',(0.163179139426149,0.281712944442145,
12.8098354422663));
#16031=CARTESIAN_POINT('Ctrl Pts',(-0.148404496997968,0.289508342399459,
12.8257276297663));
#16032=CARTESIAN_POINT('Ctrl Pts',(-0.323777087186656,0.0321293240009572,
12.8416198172663));
#16033=CARTESIAN_POINT('Ctrl Pts',(-0.202333410269313,-0.254847276161248,
12.8575120047663));
#16034=CARTESIAN_POINT('Ctrl Pts',(0.104667850400066,-0.308079814416429,
12.8734041922663));
#16035=CARTESIAN_POINT('Ctrl Pts',(0.315680507127931,-0.0788562599340915,
12.8892963797663));
#16036=CARTESIAN_POINT('Ctrl Pts',(0.23724300196989,0.222688693121784,12.9051885672663));
#16037=CARTESIAN_POINT('Ctrl Pts',(-0.0587337964425541,0.320035713812314,
12.9210807547663));
#16038=CARTESIAN_POINT('Ctrl Pts',(-0.30085395971568,0.123935386210534,
12.9369729422663));
#16039=CARTESIAN_POINT('Ctrl Pts',(-0.267112331125525,-0.185807033150192,
12.9528651297663));
#16040=CARTESIAN_POINT('Ctrl Pts',(0.0115535565262634,-0.325176177129073,
12.9687573172663));
#16041=CARTESIAN_POINT('Ctrl Pts',(0.279625421169357,-0.166381282653381,
12.9846495047663));
#16042=CARTESIAN_POINT('Ctrl Pts',(0.29129987588177,0.144974139626918,13.0005416922663));
#16043=CARTESIAN_POINT('Ctrl Pts',(0.0358720976817757,0.323398032624307,
13.0164338797663));
#16044=CARTESIAN_POINT('Ctrl Pts',(-0.252447933545031,0.205287957799053,
13.0323260672663));
#16045=CARTESIAN_POINT('Ctrl Pts',(-0.309290379226063,-0.101057243800857,
13.0482182547663));
#16046=CARTESIAN_POINT('Ctrl Pts',(-0.0825345641528824,-0.314739810610588,
13.0641104422663));
#16047=CARTESIAN_POINT('Ctrl Pts',(0.219899833900083,-0.239827369048737,
13.0800026297663));
#16048=CARTESIAN_POINT('Ctrl Pts',(0.32070103192151,0.0549904716270394,
13.0958948172663));
#16049=CARTESIAN_POINT('Ctrl Pts',(0.127441180881627,0.299385786229297,
13.1117870047663));
#16050=CARTESIAN_POINT('Ctrl Pts',(-0.182673570652711,0.269264684497214,
13.1276791922663));
#16051=CARTESIAN_POINT('Ctrl Pts',(-0.325289074233592,-0.00775383150797187,
13.1435713797663));
#16052=CARTESIAN_POINT('Ctrl Pts',(-0.16963660630581,-0.27766261087148,
13.1594635672663));
#16053=CARTESIAN_POINT('Ctrl Pts',(0.141561099453268,-0.292973648713298,
13.1753557547663));
#16054=CARTESIAN_POINT('Ctrl Pts',(0.322956898926121,-0.0396477637253095,
13.1912479422663));
#16055=CARTESIAN_POINT('Ctrl Pts',(0.208223173016264,0.250032425496528,
13.2071401297663));
#16056=CARTESIAN_POINT('Ctrl Pts',(-0.0974370493668332,0.310449875593422,
13.2230323172663));
#16057=CARTESIAN_POINT('Ctrl Pts',(-0.313754121045401,0.0862058897126582,
13.2389245047663));
#16058=CARTESIAN_POINT('Ctrl Pts',(-0.242379987620132,-0.217083035413547,
13.2548166922663));
#16059=CARTESIAN_POINT('Ctrl Pts',(0.0512401164822056,-0.321321576725432,
13.2707088797663));
#16060=CARTESIAN_POINT('Ctrl Pts',(0.29787652392791,-0.130930062480268,
13.2866010672663));
#16061=CARTESIAN_POINT('Ctrl Pts',(0.271380390078243,0.179515399836181,
13.3024932547663));
#16062=CARTESIAN_POINT('Ctrl Pts',(-0.00395308435629426,0.325357483352345,
13.3183854422663));
#16063=CARTESIAN_POINT('Ctrl Pts',(-0.275661914389586,0.172868783580475,
13.3342776297663));
#16064=CARTESIAN_POINT('Ctrl Pts',(-0.294607370647773,-0.138128664659764,
13.3501698172663));
#16065=CARTESIAN_POINT('Ctrl Pts',(-0.0434181707327341,-0.322471880103695,
13.3660620047663));
#16066=CARTESIAN_POINT('Ctrl Pts',(0.247583115853149,-0.211129547378391,
13.3819541922663));
#16067=CARTESIAN_POINT('Ctrl Pts',(0.311566325082764,0.0938026760510299,
13.3978463797663));
#16068=CARTESIAN_POINT('Ctrl Pts',(0.0898668454060592,0.312727431039774,
13.4137385672663));
#16069=CARTESIAN_POINT('Ctrl Pts',(-0.214239492875801,0.244895757422746,
13.4296307547663));
#16070=CARTESIAN_POINT('Ctrl Pts',(-0.321892306148703,-0.0474749849973848,
13.4455229422663));
#16071=CARTESIAN_POINT('Ctrl Pts',(-0.1344133836133,-0.296342682352107,
13.4614151297663));
#16072=CARTESIAN_POINT('Ctrl Pts',(0.17635816329528,-0.273425847144979,
13.4773073172663));
#16073=CARTESIAN_POINT('Ctrl Pts',(0.325329015196348,8.31833917395924E-5,
13.4931995047663));
#16074=CARTESIAN_POINT('Ctrl Pts',(0.17618765635501,0.273765455012591,13.5090916922663));
#16075=CARTESIAN_POINT('Ctrl Pts',(-0.134894208567015,0.295902967650323,
13.5249838797663));
#16076=CARTESIAN_POINT('Ctrl Pts',(-0.259001074134504,0.130532621694478,
13.535578671433));
#16077=CARTESIAN_POINT('Ctrl Pts',(-0.272283095673206,0.0399045011670809,
13.5408760672663));
#16078=CARTESIAN_POINT('Ctrl Pts',(0.148738611075541,-0.208582659521583,
12.7890255336332));
#16079=CARTESIAN_POINT('Ctrl Pts',(0.218164347404524,-0.159075727266742,
12.7943229294665));
#16080=CARTESIAN_POINT('Ctrl Pts',(0.30241420165783,0.0139851347439006,
12.8049177211332));
#16081=CARTESIAN_POINT('Ctrl Pts',(0.151907855259627,0.262254166430683,
12.8208099086331));
#16082=CARTESIAN_POINT('Ctrl Pts',(-0.138153742746315,0.269511112316996,
12.8367020961332));
#16083=CARTESIAN_POINT('Ctrl Pts',(-0.301412809686951,0.0299100529460499,
12.8525942836332));
#16084=CARTESIAN_POINT('Ctrl Pts',(-0.188357620400908,-0.237244192343189,
12.8684864711332));
#16085=CARTESIAN_POINT('Ctrl Pts',(0.0974381206128715,-0.286799795742055,
12.8843786586331));
#16086=CARTESIAN_POINT('Ctrl Pts',(0.293875485271686,-0.0734094159493023,
12.9002708461332));
#16087=CARTESIAN_POINT('Ctrl Pts',(0.220855899420353,0.207306901370254,
12.9161630336331));
#16088=CARTESIAN_POINT('Ctrl Pts',(-0.0546768727928118,0.297929864458655,
12.9320552211332));
#16089=CARTESIAN_POINT('Ctrl Pts',(-0.280073053010915,0.115374788568095,
12.9479474086332));
#16090=CARTESIAN_POINT('Ctrl Pts',(-0.248662062303876,-0.172972770890084,
12.9638395961331));
#16091=CARTESIAN_POINT('Ctrl Pts',(0.0107555169042914,-0.302715260191442,
12.9797317836332));
#16092=CARTESIAN_POINT('Ctrl Pts',(0.260310834799636,-0.154888816622663,
12.9956239711332));
#16093=CARTESIAN_POINT('Ctrl Pts',(0.271178899081166,0.134960330691056,
13.0115161586332));
#16094=CARTESIAN_POINT('Ctrl Pts',(0.0333943017573545,0.301059937587029,
13.0274083461332));
#16095=CARTESIAN_POINT('Ctrl Pts',(-0.235010579688137,0.191108088261468,
13.0433005336332));
#16096=CARTESIAN_POINT('Ctrl Pts',(-0.287926743123509,-0.0940769096970587,
13.0591927211332));
#16097=CARTESIAN_POINT('Ctrl Pts',(-0.0768336484022617,-0.292999765551001,
13.0750849086331));
#16098=CARTESIAN_POINT('Ctrl Pts',(0.204710677217587,-0.223261756330323,
13.0909770961332));
#16099=CARTESIAN_POINT('Ctrl Pts',(0.298549227003333,0.0511921109153762,
13.1068692836332));
#16100=CARTESIAN_POINT('Ctrl Pts',(0.118638427237469,0.278706290774946,
13.1227614711331));
#16101=CARTESIAN_POINT('Ctrl Pts',(-0.170055746267924,0.250665746019845,
13.1386536586332));
#16102=CARTESIAN_POINT('Ctrl Pts',(-0.302820359146324,-0.00721825055924952,
13.1545458461331));
#16103=CARTESIAN_POINT('Ctrl Pts',(-0.15791928507565,-0.258483601835419,
13.1704380336332));
#16104=CARTESIAN_POINT('Ctrl Pts',(0.131783039681204,-0.272737059284262,
13.1863302211331));
#16105=CARTESIAN_POINT('Ctrl Pts',(0.300649274347783,-0.0369091709548933,
13.2022224086332));
#16106=CARTESIAN_POINT('Ctrl Pts',(0.193840559151681,0.232761918196841,
13.2181145961331));
#16107=CARTESIAN_POINT('Ctrl Pts',(-0.0907067732076193,0.289006149516791,
13.2340067836332));
#16108=CARTESIAN_POINT('Ctrl Pts',(-0.292082160590429,0.0802513842336103,
13.2498989711331));
#16109=CARTESIAN_POINT('Ctrl Pts',(-0.225638057699727,-0.202088443650888,
13.2657911586332));
#16110=CARTESIAN_POINT('Ctrl Pts',(0.0477008043150527,-0.299126908872399,
13.2816833461332));
#16111=CARTESIAN_POINT('Ctrl Pts',(0.277301277854581,-0.121886321072234,
13.2975755336331));
#16112=CARTESIAN_POINT('Ctrl Pts',(0.252635313320574,0.167115720006175,
13.3134677211332));
#16113=CARTESIAN_POINT('Ctrl Pts',(-0.00368003268271287,0.302884043037211,
13.3293599086331));
#16114=CARTESIAN_POINT('Ctrl Pts',(-0.256621099602237,0.160928205942251,
13.3452520961332));
#16115=CARTESIAN_POINT('Ctrl Pts',(-0.274257935028732,-0.128587693697438,
13.3611442836331));
#16116=CARTESIAN_POINT('Ctrl Pts',(-0.0404191443740934,-0.300197757264567,
13.3770364711332));
#16117=CARTESIAN_POINT('Ctrl Pts',(0.230481789890607,-0.196546181313221,
13.3929286586331));
#16118=CARTESIAN_POINT('Ctrl Pts',(0.290045482412086,0.0873234372152981,
13.4088208461332));
#16119=CARTESIAN_POINT('Ctrl Pts',(0.0836594664770931,0.291126387215721,
13.4247130336331));
#16120=CARTESIAN_POINT('Ctrl Pts',(-0.199441313326708,0.227980055557946,
13.4406052211332));
#16121=CARTESIAN_POINT('Ctrl Pts',(-0.299658216262103,-0.044195742021913,
13.4564974086332));
#16122=CARTESIAN_POINT('Ctrl Pts',(-0.125129038519821,-0.275873383425748,
13.4723895961332));
#16123=CARTESIAN_POINT('Ctrl Pts',(0.164176563486767,-0.254539484387576,
13.4882817836332));
#16124=CARTESIAN_POINT('Ctrl Pts',(0.302857541264153,7.7437659476318E-5,
13.5041739711332));
#16125=CARTESIAN_POINT('Ctrl Pts',(0.164017833984366,0.25485563449708,13.5200661586332));
#16126=CARTESIAN_POINT('Ctrl Pts',(-0.125576651417715,0.275464041168465,
13.5359583461332));
#16127=CARTESIAN_POINT('Ctrl Pts',(-0.241111074737091,0.121516332741775,
13.5465531377998));
#16128=CARTESIAN_POINT('Ctrl Pts',(-0.253475666268531,0.0371481747533046,
13.5518505336332));
#16129=CARTESIAN_POINT('Ctrl Pts',(0.137702479013109,-0.19310620885576,
12.8));
#16130=CARTESIAN_POINT('Ctrl Pts',(0.201976953076579,-0.147272600147639,
12.8052973958333));
#16131=CARTESIAN_POINT('Ctrl Pts',(0.279975622711063,0.012947463403363,
12.8158921875));
#16132=CARTESIAN_POINT('Ctrl Pts',(0.140636571093104,0.242795388419221,
12.831784375));
#16133=CARTESIAN_POINT('Ctrl Pts',(-0.127902988494662,0.249513882234533,
12.8476765625));
#16134=CARTESIAN_POINT('Ctrl Pts',(-0.279048532187246,0.0276907818911422,
12.86356875));
#16135=CARTESIAN_POINT('Ctrl Pts',(-0.174381830532504,-0.219641108525129,
12.8794609375));
#16136=CARTESIAN_POINT('Ctrl Pts',(0.0902083908256771,-0.26551977706768,
12.895353125));
#16137=CARTESIAN_POINT('Ctrl Pts',(0.27207046341544,-0.0679625719645133,
12.9112453125));
#16138=CARTESIAN_POINT('Ctrl Pts',(0.204468796870817,0.191925109618724,
12.9271375));
#16139=CARTESIAN_POINT('Ctrl Pts',(-0.0506199491430696,0.275824015104995,
12.9430296875));
#16140=CARTESIAN_POINT('Ctrl Pts',(-0.25929214630615,0.106814190925657,
12.958921875));
#16141=CARTESIAN_POINT('Ctrl Pts',(-0.230211793482226,-0.160138508629975,
12.9748140625));
#16142=CARTESIAN_POINT('Ctrl Pts',(0.00995747728231949,-0.28025434325381,
12.99070625));
#16143=CARTESIAN_POINT('Ctrl Pts',(0.240996248429915,-0.143396350591946,
13.0065984375));
#16144=CARTESIAN_POINT('Ctrl Pts',(0.251057922280563,0.124946521755194,
13.022490625));
#16145=CARTESIAN_POINT('Ctrl Pts',(0.0309165058329335,0.27872184254975,
13.0383828125));
#16146=CARTESIAN_POINT('Ctrl Pts',(-0.217573225831243,0.176928218723883,
13.054275));
#16147=CARTESIAN_POINT('Ctrl Pts',(-0.266563107020954,-0.0870965755932605,
13.0701671875));
#16148=CARTESIAN_POINT('Ctrl Pts',(-0.0711327326516408,-0.271259720491414,
13.086059375));
#16149=CARTESIAN_POINT('Ctrl Pts',(0.189521520535091,-0.206696143611909,
13.1019515625));
#16150=CARTESIAN_POINT('Ctrl Pts',(0.276397422085156,0.0473937502037132,
13.11784375));
#16151=CARTESIAN_POINT('Ctrl Pts',(0.109835673593312,0.258026795320596,
13.1337359375));
#16152=CARTESIAN_POINT('Ctrl Pts',(-0.157437921883138,0.232066807542476,
13.149628125));
#16153=CARTESIAN_POINT('Ctrl Pts',(-0.280351644059057,-0.00668266961052725,
13.1655203125));
#16154=CARTESIAN_POINT('Ctrl Pts',(-0.14620196384549,-0.239304592799359,
13.1814125));
#16155=CARTESIAN_POINT('Ctrl Pts',(0.12200497990914,-0.252500469855226,
13.1973046875));
#16156=CARTESIAN_POINT('Ctrl Pts',(0.278341649769444,-0.034170578184477,
13.213196875));
#16157=CARTESIAN_POINT('Ctrl Pts',(0.179457945287098,0.215491410897154,
13.2290890625));
#16158=CARTESIAN_POINT('Ctrl Pts',(-0.0839764970484053,0.267562423440159,
13.24498125));
#16159=CARTESIAN_POINT('Ctrl Pts',(-0.270410200135457,0.0742968787545624,
13.2608734375));
#16160=CARTESIAN_POINT('Ctrl Pts',(-0.208896127779322,-0.18709385188823,
13.276765625));
#16161=CARTESIAN_POINT('Ctrl Pts',(0.0441614921479,-0.276932241019365,13.2926578125));
#16162=CARTESIAN_POINT('Ctrl Pts',(0.256726031781252,-0.1128425796642,13.30855));
#16163=CARTESIAN_POINT('Ctrl Pts',(0.233890236562906,0.154716040176168,
13.3244421875));
#16164=CARTESIAN_POINT('Ctrl Pts',(-0.00340698100913133,0.280410602722076,
13.340334375));
#16165=CARTESIAN_POINT('Ctrl Pts',(-0.237580284814888,0.148987628304026,
13.3562265625));
#16166=CARTESIAN_POINT('Ctrl Pts',(-0.253908499409691,-0.119046722735112,
13.37211875));
#16167=CARTESIAN_POINT('Ctrl Pts',(-0.0374201180154527,-0.277923634425439,
13.3880109375));
#16168=CARTESIAN_POINT('Ctrl Pts',(0.213380463928066,-0.18196281524805,
13.403903125));
#16169=CARTESIAN_POINT('Ctrl Pts',(0.268524639741408,0.0808441983795663,
13.4197953125));
#16170=CARTESIAN_POINT('Ctrl Pts',(0.077452087548127,0.269525343391667,
13.4356875));
#16171=CARTESIAN_POINT('Ctrl Pts',(-0.184643133777616,0.211064353693145,
13.4515796875));
#16172=CARTESIAN_POINT('Ctrl Pts',(-0.277424126375503,-0.0409164990464411,
13.467471875));
#16173=CARTESIAN_POINT('Ctrl Pts',(-0.115844693426342,-0.255404084499389,
13.4833640625));
#16174=CARTESIAN_POINT('Ctrl Pts',(0.151994963678255,-0.235653121630174,
13.49925625));
#16175=CARTESIAN_POINT('Ctrl Pts',(0.280386067331958,7.16919272130007E-5,
13.5151484375));
#16176=CARTESIAN_POINT('Ctrl Pts',(0.151848011613721,0.23594581398157,13.531040625));
#16177=CARTESIAN_POINT('Ctrl Pts',(-0.116259094268414,0.255025114686607,
13.5469328125));
#16178=CARTESIAN_POINT('Ctrl Pts',(-0.223221075339677,0.112500043789072,
13.5575276041667));
#16179=CARTESIAN_POINT('Ctrl Pts',(-0.234668236863856,0.0343918483395283,
13.562825));
#16180=CARTESIAN_POINT('',(0.137702479013109,-0.19310620885576,12.8));
#16181=CARTESIAN_POINT('Ctrl Pts',(0.137702479013109,-0.19310620885576,
12.8));
#16182=CARTESIAN_POINT('Ctrl Pts',(0.201976953076579,-0.147272600147639,
12.8052973958333));
#16183=CARTESIAN_POINT('Ctrl Pts',(0.279975622711063,0.012947463403363,
12.8158921875));
#16184=CARTESIAN_POINT('Ctrl Pts',(0.140636571093104,0.242795388419221,
12.831784375));
#16185=CARTESIAN_POINT('Ctrl Pts',(-0.127902988494662,0.249513882234533,
12.8476765625));
#16186=CARTESIAN_POINT('Ctrl Pts',(-0.233651108552229,0.0943166116198947,
12.8587954411032));
#16187=CARTESIAN_POINT('Ctrl Pts',(-0.237528617395594,0.0079260774111979,
12.864616923873));
#16188=CARTESIAN_POINT('Ctrl Pts',(-0.237475867347687,0.000143668378376506,
12.8651410108095));
#16189=CARTESIAN_POINT('Ctrl Pts',(0.129215683242003,0.264846751495042,
12.8));
#16190=CARTESIAN_POINT('Ctrl Pts',(0.135212459169762,0.261232067552344,
12.8));
#16191=CARTESIAN_POINT('Ctrl Pts',(0.141061626425574,0.257394031435174,
12.8));
#16192=CARTESIAN_POINT('Ctrl Pts',(0.146748920713232,0.253331893839978,
12.8));
#16193=CARTESIAN_POINT('Ctrl Pts',(0.15657328667399,0.246314861785777,12.8));
#16194=CARTESIAN_POINT('Ctrl Pts',(0.165915195693812,0.238629441830809,
12.8));
#16195=CARTESIAN_POINT('Ctrl Pts',(0.174740580578172,0.230346357604821,
12.8));
#16196=CARTESIAN_POINT('Ctrl Pts',(0.178901236248919,0.226441365153193,
12.8));
#16197=CARTESIAN_POINT('Ctrl Pts',(0.182946948479838,0.222403433701439,
12.8));
#16198=CARTESIAN_POINT('Ctrl Pts',(0.186873336456426,0.218239549379721,
12.8));
#16199=CARTESIAN_POINT('Ctrl Pts',(0.190449962393121,0.214446583235962,
12.8));
#16200=CARTESIAN_POINT('Ctrl Pts',(0.193924720399342,0.210551920535541,
12.8));
#16201=CARTESIAN_POINT('Ctrl Pts',(0.197289746551245,0.206567301120756,
12.8));
#16202=CARTESIAN_POINT('Ctrl Pts',(0.20843723213549,0.193367258838793,12.8));
#16203=CARTESIAN_POINT('Ctrl Pts',(0.218402335066749,0.179162279576202,
12.8));
#16204=CARTESIAN_POINT('Ctrl Pts',(0.227068433305708,0.164154641391987,
12.8));
#16205=CARTESIAN_POINT('Ctrl Pts',(0.230494359574639,0.158221745125157,
12.8));
#16206=CARTESIAN_POINT('Ctrl Pts',(0.233718830599218,0.152158127352311,
12.8));
#16207=CARTESIAN_POINT('Ctrl Pts',(0.236719485594126,0.146004799286039,
12.8));
#16208=CARTESIAN_POINT('Ctrl Pts',(0.244057081504557,0.130957872887894,
12.8));
#16209=CARTESIAN_POINT('Ctrl Pts',(0.250077313467251,0.115349535038238,
12.8));
#16210=CARTESIAN_POINT('Ctrl Pts',(0.254672578472357,0.0993652496009151,
12.8));
#16211=CARTESIAN_POINT('Ctrl Pts',(0.257632497295663,0.0890693934771714,
12.8));
#16212=CARTESIAN_POINT('Ctrl Pts',(0.260000238425513,0.0786172356827657,
12.8));
#16213=CARTESIAN_POINT('Ctrl Pts',(0.261735268122606,0.0680587419952843,
12.8));
#16214=CARTESIAN_POINT('Ctrl Pts',(0.26247802203292,0.0635387257174422,
12.8));
#16215=CARTESIAN_POINT('Ctrl Pts',(0.263104701090492,0.0589992464261977,
12.8));
#16216=CARTESIAN_POINT('Ctrl Pts',(0.263611560734367,0.0544443848764751,
12.8));
#16217=CARTESIAN_POINT('Ctrl Pts',(0.264100883204341,0.0500471200106794,
12.8));
#16218=CARTESIAN_POINT('Ctrl Pts',(0.264477472227069,0.0456446896458848,
12.8));
#16219=CARTESIAN_POINT('Ctrl Pts',(0.264739070133745,0.0412429691345073,
12.8));
#16220=CARTESIAN_POINT('Ctrl Pts',(0.265309177961261,0.0316501732671333,
12.8));
#16221=CARTESIAN_POINT('Ctrl Pts',(0.2653340197788,0.0220570104352547,12.8));
#16222=CARTESIAN_POINT('Ctrl Pts',(0.264787883227811,0.0125003360521388,
12.8));
#16223=CARTESIAN_POINT('Ctrl Pts',(0.263862534527666,-0.003692054298092,
12.8));
#16224=CARTESIAN_POINT('Ctrl Pts',(0.261300185398629,-0.019781536702279,
12.8));
#16225=CARTESIAN_POINT('Ctrl Pts',(0.257203559968843,-0.0355693262937758,
12.8));
#16226=CARTESIAN_POINT('Ctrl Pts',(0.256089106652214,-0.0398642648411328,
12.8));
#16227=CARTESIAN_POINT('Ctrl Pts',(0.254860056647025,-0.0441391928129072,
12.8));
#16228=CARTESIAN_POINT('Ctrl Pts',(0.253520584007838,-0.0483814917048708,
12.8));
#16229=CARTESIAN_POINT('Ctrl Pts',(0.248750211286509,-0.063489935369865,
12.8));
#16230=CARTESIAN_POINT('Ctrl Pts',(0.242605109706018,-0.0781226040481322,
12.8));
#16231=CARTESIAN_POINT('Ctrl Pts',(0.235197469927049,-0.0921011352816676,
12.8));
#16232=CARTESIAN_POINT('Ctrl Pts',(0.229495020889561,-0.10286189908183,
12.8));
#16233=CARTESIAN_POINT('Ctrl Pts',(0.223043166859496,-0.11323484442185,
12.8));
#16234=CARTESIAN_POINT('Ctrl Pts',(0.215878086649736,-0.123123415869591,
12.8));
#16235=CARTESIAN_POINT('Ctrl Pts',(0.213283707523951,-0.126703934523508,
12.8));
#16236=CARTESIAN_POINT('Ctrl Pts',(0.210594525319483,-0.130222266390069,
12.8));
#16237=CARTESIAN_POINT('Ctrl Pts',(0.207815760318832,-0.133668560993862,
12.8));
#16238=CARTESIAN_POINT('Ctrl Pts',(0.198088582382188,-0.145732452983772,
12.8));
#16239=CARTESIAN_POINT('Ctrl Pts',(0.187325168437807,-0.156846059287663,
12.8));
#16240=CARTESIAN_POINT('Ctrl Pts',(0.175614388817618,-0.166823177757923,
12.8));
#16241=CARTESIAN_POINT('Ctrl Pts',(0.16463984863336,-0.1761730495108,12.8));
#16242=CARTESIAN_POINT('Ctrl Pts',(0.152832183702603,-0.184525367271261,
12.8));
#16243=CARTESIAN_POINT('Ctrl Pts',(0.140246050763535,-0.191682120721285,
12.8));
#16244=CARTESIAN_POINT('Ctrl Pts',(0.139401695805602,-0.192162239617811,
12.8));
#16245=CARTESIAN_POINT('Ctrl Pts',(0.138553833519603,-0.1926369584628,12.8));
#16246=CARTESIAN_POINT('Ctrl Pts',(0.137702479013111,-0.193106208855758,
12.8));
#16247=CARTESIAN_POINT('Ctrl Pts',(0.0261206201035208,0.292499143797287,
13.5058));
#16248=CARTESIAN_POINT('Ctrl Pts',(0.0734750452512648,0.288342804146702,
13.5032390752998));
#16249=CARTESIAN_POINT('Ctrl Pts',(0.119860787283314,0.273336395466611,
13.5006781505996));
#16250=CARTESIAN_POINT('Ctrl Pts',(0.159503106385806,0.247855320894766,
13.4981172258995));
#16251=CARTESIAN_POINT('Ctrl Pts',(0.24150514885995,0.195146493393404,13.4928198300661));
#16252=CARTESIAN_POINT('Ctrl Pts',(0.294652818994247,0.0976177112587029,
13.4875224342328));
#16253=CARTESIAN_POINT('Ctrl Pts',(0.294683199723937,0.000119797020287853,
13.4822250383995));
#16254=CARTESIAN_POINT('Ctrl Pts',(0.294713580453626,-0.0973781172181258,
13.4769276425661));
#16255=CARTESIAN_POINT('Ctrl Pts',(0.241626671778709,-0.194845163560254,
13.4716302467328));
#16256=CARTESIAN_POINT('Ctrl Pts',(0.159710302139489,-0.247661981960665,
13.4663328508995));
#16257=CARTESIAN_POINT('Ctrl Pts',(0.0777939325002679,-0.300478800361077,
13.4610354550661));
#16258=CARTESIAN_POINT('Ctrl Pts',(-0.0329518981032568,-0.308645390819771,
13.4557380592328));
#16259=CARTESIAN_POINT('Ctrl Pts',(-0.121729591293106,-0.268385727164849,
13.4504406633995));
#16260=CARTESIAN_POINT('Ctrl Pts',(-0.210507284482955,-0.228126063509928,
13.4451432675661));
#16261=CARTESIAN_POINT('Ctrl Pts',(-0.277316840259129,-0.139440145741392,
13.4398458717328));
#16262=CARTESIAN_POINT('Ctrl Pts',(-0.291540164212148,-0.0430029056470576,
13.4345484758995));
#16263=CARTESIAN_POINT('Ctrl Pts',(-0.293626260696475,-0.0288587162730754,
13.4337715211693));
#16264=CARTESIAN_POINT('Ctrl Pts',(-0.29458115917577,-0.0145477859091552,
13.4329945664391));
#16265=CARTESIAN_POINT('Ctrl Pts',(-0.294460332090693,-0.000220795745557084,
13.432217611709));
#16266=CARTESIAN_POINT('Origin',(0.,0.,12.6151410108095));
#16267=CARTESIAN_POINT('',(-0.13770247901312,-0.193106208855752,12.8));
#16268=CARTESIAN_POINT('Ctrl Pts',(-0.138011838534631,-0.193375383177942,
12.8));
#16269=CARTESIAN_POINT('Ctrl Pts',(-0.0781015645619646,-0.235657681198368,
12.8049405016152));
#16270=CARTESIAN_POINT('Ctrl Pts',(0.0903526836839373,-0.26250844141701,
12.8151859925577));
#16271=CARTESIAN_POINT('Ctrl Pts',(0.271186343139681,-0.0718941087923526,
12.8307364728275));
#16272=CARTESIAN_POINT('Ctrl Pts',(0.207021633736509,0.189392429248662,
12.8466514408095));
#16273=CARTESIAN_POINT('Ctrl Pts',(-0.0475028660546131,0.276509970564655,
12.8625664087915));
#16274=CARTESIAN_POINT('Ctrl Pts',(-0.216222593118796,0.142818607294397,
12.8753022582519));
#16275=CARTESIAN_POINT('Ctrl Pts',(-0.237002089177395,0.0319078962725245,
12.8827331183849));
#16276=CARTESIAN_POINT('Ctrl Pts',(-0.23685325391662,0.000124198907147644,
12.8848589891905));
#16277=CARTESIAN_POINT('Origin',(0.,0.,12.8));
#16278=CARTESIAN_POINT('Ctrl Pts',(-0.103908919352494,0.213201587949051,
12.7670766008995));
#16279=CARTESIAN_POINT('Ctrl Pts',(-0.174973765135383,0.178566426924752,
12.7723815902268));
#16280=CARTESIAN_POINT('Ctrl Pts',(-0.278449645037139,0.0331055665616523,
12.7829915688815));
#16281=CARTESIAN_POINT('Ctrl Pts',(-0.178281517311376,-0.216843324364553,
12.7989065368635));
#16282=CARTESIAN_POINT('Ctrl Pts',(0.086114123480329,-0.26697625082225,
12.8148215048455));
#16283=CARTESIAN_POINT('Ctrl Pts',(0.271186343139681,-0.0718941087923526,
12.8307364728275));
#16284=CARTESIAN_POINT('Ctrl Pts',(0.207021633736509,0.189392429248662,
12.8466514408095));
#16285=CARTESIAN_POINT('Ctrl Pts',(-0.0475028660546131,0.276509970564655,
12.8625664087915));
#16286=CARTESIAN_POINT('Ctrl Pts',(-0.258338355475561,0.109446613499621,
12.8784813767735));
#16287=CARTESIAN_POINT('Ctrl Pts',(-0.231681731794662,-0.158247829181543,
12.8943963447556));
#16288=CARTESIAN_POINT('Ctrl Pts',(0.00797328488061451,-0.280452709922419,
12.9103113127376));
#16289=CARTESIAN_POINT('Ctrl Pts',(0.240296121102423,-0.14482920233622,
12.9262262807196));
#16290=CARTESIAN_POINT('Ctrl Pts',(0.251706166281744,0.123942967091746,
12.9421412487016));
#16291=CARTESIAN_POINT('Ctrl Pts',(0.0317122558575804,0.278768752799521,
12.9580562166836));
#16292=CARTESIAN_POINT('Ctrl Pts',(-0.21743576073689,0.177311681816183,
12.9739711846656));
#16293=CARTESIAN_POINT('Ctrl Pts',(-0.266686554811307,-0.0871552256344479,
12.9898861526476));
#16294=CARTESIAN_POINT('Ctrl Pts',(-0.0707617483345123,-0.271496792539298,
13.0058011206296));
#16295=CARTESIAN_POINT('Ctrl Pts',(0.19021711870995,-0.20624060859311,13.0217160886116));
#16296=CARTESIAN_POINT('Ctrl Pts',(0.276321843237659,0.0486207800379639,
13.0376310565936));
#16297=CARTESIAN_POINT('Ctrl Pts',(0.108392911780422,0.258783144727794,
13.0535460245757));
#16298=CARTESIAN_POINT('Ctrl Pts',(-0.159185927336213,0.231035886385667,
13.0694609925577));
#16299=CARTESIAN_POINT('Ctrl Pts',(-0.280418819849278,-0.0091118443472218,
13.0853759605397));
#16300=CARTESIAN_POINT('Ctrl Pts',(-0.143851548471854,-0.240882693501056,
13.1012909285217));
#16301=CARTESIAN_POINT('Ctrl Pts',(0.124964166840451,-0.25120051183695,
13.1172058965037));
#16302=CARTESIAN_POINT('Ctrl Pts',(0.278895358440525,-0.030579718254803,
13.1331208644857));
#16303=CARTESIAN_POINT('Ctrl Pts',(0.176426965387693,0.218154225247527,
13.1490358324677));
#16304=CARTESIAN_POINT('Ctrl Pts',(-0.0882377470317194,0.266330321450576,
13.1649508004497));
#16305=CARTESIAN_POINT('Ctrl Pts',(-0.271781992573435,0.0696583707968577,
13.1808657684317));
#16306=CARTESIAN_POINT('Ctrl Pts',(-0.205466253473662,-0.191053287885107,
13.1967807364137));
#16307=CARTESIAN_POINT('Ctrl Pts',(0.0497427765240963,-0.276122067797826,
13.2126957043958));
#16308=CARTESIAN_POINT('Ctrl Pts',(0.259221295320457,-0.107340859314887,
13.2286106723778));
#16309=CARTESIAN_POINT('Ctrl Pts',(0.23038737805747,0.160123065998856,13.2445256403598));
#16310=CARTESIAN_POINT('Ctrl Pts',(-0.0102508111899536,0.280379494845555,
13.2604406083418));
#16311=CARTESIAN_POINT('Ctrl Pts',(-0.241465019981373,0.14287191272199,
13.2763555763238));
#16312=CARTESIAN_POINT('Ctrl Pts',(-0.250690846589451,-0.125983493910996,
13.2922705443058));
#16313=CARTESIAN_POINT('Ctrl Pts',(-0.0294466067184147,-0.279017272289624,
13.3081855122878));
#16314=CARTESIAN_POINT('Ctrl Pts',(0.218869047461476,-0.175539378629952,
13.3241004802698));
#16315=CARTESIAN_POINT('Ctrl Pts',(0.265969733682413,0.0893188257727471,
13.3400154482518));
#16316=CARTESIAN_POINT('Ctrl Pts',(0.0685537852907199,0.272062715339731,
13.3559304162339));
#16317=CARTESIAN_POINT('Ctrl Pts',(-0.191886195286831,0.204688477368222,
13.3718453842159));
#16318=CARTESIAN_POINT('Ctrl Pts',(-0.275917956826614,-0.0508638804691982,
13.3877603521979));
#16319=CARTESIAN_POINT('Ctrl Pts',(-0.106286584194727,-0.259655320928406,
13.4036753201799));
#16320=CARTESIAN_POINT('Ctrl Pts',(0.161056632784338,-0.229734753162831,
13.4195902881619));
#16321=CARTESIAN_POINT('Ctrl Pts',(0.280337460803119,0.0113889577443968,
13.4355052561439));
#16322=CARTESIAN_POINT('Ctrl Pts',(0.141885966824002,0.242044705653255,
13.4514202241259));
#16323=CARTESIAN_POINT('Ctrl Pts',(-0.126992591218768,0.250174275017661,
13.4673351921079));
#16324=CARTESIAN_POINT('Ctrl Pts',(-0.279151391016313,0.0283187214630216,
13.4832501600899));
#16325=CARTESIAN_POINT('Ctrl Pts',(-0.17461423217311,-0.219592043360215,
13.499165128072));
#16326=CARTESIAN_POINT('Ctrl Pts',(0.0903269506402298,-0.265580501456578,
13.515080096054));
#16327=CARTESIAN_POINT('Ctrl Pts',(0.272486967933624,-0.0674994743880085,
13.530995064036));
#16328=CARTESIAN_POINT('Ctrl Pts',(0.203600577200948,0.19281335099551,13.546910032018));
#16329=CARTESIAN_POINT('Ctrl Pts',(0.0337423613347716,0.2477160478489,13.5575200106727));
#16330=CARTESIAN_POINT('Ctrl Pts',(-0.043944522199392,0.233068358199193,
13.562825));
#16331=CARTESIAN_POINT('Ctrl Pts',(-0.112236674703431,0.230288577939276,
12.7780510672663));
#16332=CARTESIAN_POINT('Ctrl Pts',(-0.18899699546017,0.192877590264599,
12.7833560565936));
#16333=CARTESIAN_POINT('Ctrl Pts',(-0.300765924870234,0.0357588042316975,
12.7939660352483));
#16334=CARTESIAN_POINT('Ctrl Pts',(-0.19256984663878,-0.234222180443943,
12.8098810032303));
#16335=CARTESIAN_POINT('Ctrl Pts',(0.0930157191958205,-0.288372998235396,
12.8257959712123));
#16336=CARTESIAN_POINT('Ctrl Pts',(0.292920507389061,-0.0776560448506564,
12.8417109391944));
#16337=CARTESIAN_POINT('Ctrl Pts',(0.223613332782678,0.204571239941054,
12.8576259071764));
#16338=CARTESIAN_POINT('Ctrl Pts',(-0.0513099718299037,0.298670795653654,
12.8735408751584));
#16339=CARTESIAN_POINT('Ctrl Pts',(-0.279042820843599,0.118218186016141,
12.8894558431404));
#16340=CARTESIAN_POINT('Ctrl Pts',(-0.250249808468835,-0.170930563391974,
12.9053708111224));
#16341=CARTESIAN_POINT('Ctrl Pts',(0.00861230187975927,-0.302929524908998,
12.9212857791044));
#16342=CARTESIAN_POINT('Ctrl Pts',(0.259554595935866,-0.156436503925375,
12.9372007470864));
#16343=CARTESIAN_POINT('Ctrl Pts',(0.271879096441916,0.133876346380466,
12.9531157150684));
#16344=CARTESIAN_POINT('Ctrl Pts',(0.0342538269763452,0.301110607447485,
12.9690306830504));
#16345=CARTESIAN_POINT('Ctrl Pts',(-0.234862097486857,0.191522283911076,
12.9849456510324));
#16346=CARTESIAN_POINT('Ctrl Pts',(-0.28806008460733,-0.0941402602316915,
13.0008606190145));
#16347=CARTESIAN_POINT('Ctrl Pts',(-0.0764329316362602,-0.293255837681146,
13.0167755869965));
#16348=CARTESIAN_POINT('Ctrl Pts',(0.205462023940876,-0.222769712567,13.0326905549785));
#16349=CARTESIAN_POINT('Ctrl Pts',(0.298467590907281,0.0525174807605868,
13.0486055229605));
#16350=CARTESIAN_POINT('Ctrl Pts',(0.117080035626076,0.279523257623478,
13.0645204909425));
#16351=CARTESIAN_POINT('Ctrl Pts',(-0.171943845197633,0.249552201934865,
13.0804354589245));
#16352=CARTESIAN_POINT('Ctrl Pts',(-0.302892918724096,-0.00984211092098895,
13.0963504269065));
#16353=CARTESIAN_POINT('Ctrl Pts',(-0.155380496227179,-0.260188179038313,
13.1122653948885));
#16354=CARTESIAN_POINT('Ctrl Pts',(0.134979389937427,-0.271332916443256,
13.1281803628705));
#16355=CARTESIAN_POINT('Ctrl Pts',(0.301247359867139,-0.0330305224197738,
13.1440953308526));
#16356=CARTESIAN_POINT('Ctrl Pts',(0.190566662097203,0.235638143162905,
13.1600102988346));
#16357=CARTESIAN_POINT('Ctrl Pts',(-0.095309540045996,0.287675301009579,
13.1759252668166));
#16358=CARTESIAN_POINT('Ctrl Pts',(-0.293563895003427,0.0752411241712175,
13.1918402347986));
#16359=CARTESIAN_POINT('Ctrl Pts',(-0.22193329694274,-0.206365207693472,
13.2077552027806));
#16360=CARTESIAN_POINT('Ctrl Pts',(0.0537293993852549,-0.298251804512869,
13.2236701707626));
#16361=CARTESIAN_POINT('Ctrl Pts',(0.279996523690013,-0.115943666668714,
13.2395851387446));
#16362=CARTESIAN_POINT('Ctrl Pts',(0.248851719062674,0.172956090613008,
13.2555001067266));
#16363=CARTESIAN_POINT('Ctrl Pts',(-0.0110723599874049,0.302850442027407,
13.2714150747086));
#16364=CARTESIAN_POINT('Ctrl Pts',(-0.260817175934343,0.15432234780575,
13.2873300426906));
#16365=CARTESIAN_POINT('Ctrl Pts',(-0.270782404197074,-0.136080410730889,
13.3032450106727));
#16366=CARTESIAN_POINT('Ctrl Pts',(-0.0318065979318202,-0.301379044472352,
13.3191599786547));
#16367=CARTESIAN_POINT('Ctrl Pts',(0.236410254631274,-0.189607939912231,
13.3350749466367));
#16368=CARTESIAN_POINT('Ctrl Pts',(0.287285814021459,0.096477261582719,
13.3509899146187));
#16369=CARTESIAN_POINT('Ctrl Pts',(0.0740480119253485,0.293867116228312,
13.3669048826007));
#16370=CARTESIAN_POINT('Ctrl Pts',(-0.20726486825859,0.221093186158389,
13.3828198505827));
#16371=CARTESIAN_POINT('Ctrl Pts',(-0.298031335116959,-0.0549403539364065,
13.3987348185647));
#16372=CARTESIAN_POINT('Ctrl Pts',(-0.114804896922607,-0.280465334175926,
13.4146497865467));
#16373=CARTESIAN_POINT('Ctrl Pts',(0.173964477883985,-0.248146789702814,
13.4305647545288));
#16374=CARTESIAN_POINT('Ctrl Pts',(0.302805039176751,0.0123017230237244,
13.4464797225107));
#16375=CARTESIAN_POINT('Ctrl Pts',(0.153257383510892,0.261443320374982,
13.4623946904928));
#16376=CARTESIAN_POINT('Ctrl Pts',(-0.137170381899699,0.2702244321209,13.4783096584748));
#16377=CARTESIAN_POINT('Ctrl Pts',(-0.301523912112135,0.030588318583895,
13.4942246264568));
#16378=CARTESIAN_POINT('Ctrl Pts',(-0.188608647815107,-0.237191194862433,
13.5101395944388));
#16379=CARTESIAN_POINT('Ctrl Pts',(0.0975661823752476,-0.286865386872497,
13.5260545624208));
#16380=CARTESIAN_POINT('Ctrl Pts',(0.294325370444308,-0.0729092035289056,
13.5419695304028));
#16381=CARTESIAN_POINT('Ctrl Pts',(0.219918096493853,0.208266330638556,
13.5578844983848));
#16382=CARTESIAN_POINT('Ctrl Pts',(0.0364466347687562,0.267569190926913,
13.5684944770395));
#16383=CARTESIAN_POINT('Ctrl Pts',(-0.0474664453622039,0.251747565713066,
13.5737994663668));
#16384=CARTESIAN_POINT('Ctrl Pts',(-0.120564430054368,0.247375567929501,
12.7890255336332));
#16385=CARTESIAN_POINT('Ctrl Pts',(-0.203020225784959,0.207188753604445,
12.7943305229605));
#16386=CARTESIAN_POINT('Ctrl Pts',(-0.323082204703329,0.0384120419017428,
12.8049405016152));
#16387=CARTESIAN_POINT('Ctrl Pts',(-0.206858175966185,-0.251601036523333,
12.8208554695972));
#16388=CARTESIAN_POINT('Ctrl Pts',(0.0999173149113121,-0.309769745648542,
12.8367704375792));
#16389=CARTESIAN_POINT('Ctrl Pts',(0.314654671638441,-0.0834179809089602,
12.8526854055612));
#16390=CARTESIAN_POINT('Ctrl Pts',(0.240205031828846,0.219750050633447,
12.8686003735432));
#16391=CARTESIAN_POINT('Ctrl Pts',(-0.0551170776051942,0.320831620742652,
12.8845153415252));
#16392=CARTESIAN_POINT('Ctrl Pts',(-0.299747286211637,0.12698975853266,
12.9004303095072));
#16393=CARTESIAN_POINT('Ctrl Pts',(-0.268817885143008,-0.183613297602405,
12.9163452774892));
#16394=CARTESIAN_POINT('Ctrl Pts',(0.00925131887890369,-0.325406339895578,
12.9322602454712));
#16395=CARTESIAN_POINT('Ctrl Pts',(0.278813070769308,-0.16804380551453,
12.9481752134533));
#16396=CARTESIAN_POINT('Ctrl Pts',(0.292052026602089,0.143809725669185,
12.9640901814353));
#16397=CARTESIAN_POINT('Ctrl Pts',(0.0367953980951103,0.323452462095449,
12.9800051494173));
#16398=CARTESIAN_POINT('Ctrl Pts',(-0.252288434236825,0.205732886005968,
12.9959201173993));
#16399=CARTESIAN_POINT('Ctrl Pts',(-0.309433614403352,-0.101125294828935,
13.0118350853813));
#16400=CARTESIAN_POINT('Ctrl Pts',(-0.0821041149380083,-0.315014882822994,
13.0277500533633));
#16401=CARTESIAN_POINT('Ctrl Pts',(0.220706929171802,-0.239298816540891,
13.0436650213453));
#16402=CARTESIAN_POINT('Ctrl Pts',(0.320613338576903,0.0564141814832096,
13.0595799893273));
#16403=CARTESIAN_POINT('Ctrl Pts',(0.125767159471731,0.300263370519163,
13.0754949573094));
#16404=CARTESIAN_POINT('Ctrl Pts',(-0.184701763059053,0.268068517484062,
13.0914099252914));
#16405=CARTESIAN_POINT('Ctrl Pts',(-0.325367017598915,-0.010572377494756,
13.1073248932734));
#16406=CARTESIAN_POINT('Ctrl Pts',(-0.166909443982505,-0.279493664575571,
13.1232398612554));
#16407=CARTESIAN_POINT('Ctrl Pts',(0.144994613034403,-0.291465321049563,
13.1391548292374));
#16408=CARTESIAN_POINT('Ctrl Pts',(0.323599361293752,-0.0354813265847442,
13.1550697972194));
#16409=CARTESIAN_POINT('Ctrl Pts',(0.204706358806712,0.253122061078283,
13.1709847652014));
#16410=CARTESIAN_POINT('Ctrl Pts',(-0.102381333060272,0.309020280568582,
13.1868997331834));
#16411=CARTESIAN_POINT('Ctrl Pts',(-0.315345797433419,0.0808238775455775,
13.2028147011654));
#16412=CARTESIAN_POINT('Ctrl Pts',(-0.238400340411818,-0.221677127501839,
13.2187296691474));
#16413=CARTESIAN_POINT('Ctrl Pts',(0.0577160222464135,-0.320381541227913,
13.2346446371294));
#16414=CARTESIAN_POINT('Ctrl Pts',(0.30077175205957,-0.124546474022541,
13.2505596051115));
#16415=CARTESIAN_POINT('Ctrl Pts',(0.267316060067878,0.185789115227159,
13.2664745730935));
#16416=CARTESIAN_POINT('Ctrl Pts',(-0.0118939087848559,0.32532138920926,
13.2823895410755));
#16417=CARTESIAN_POINT('Ctrl Pts',(-0.280169331887314,0.16577278288951,
13.2983045090575));
#16418=CARTESIAN_POINT('Ctrl Pts',(-0.290873961804697,-0.146177327550781,
13.3142194770395));
#16419=CARTESIAN_POINT('Ctrl Pts',(-0.0341665891452253,-0.323740816655081,
13.3301344450215));
#16420=CARTESIAN_POINT('Ctrl Pts',(0.253951461801071,-0.20367650119451,
13.3460494130035));
#16421=CARTESIAN_POINT('Ctrl Pts',(0.308601894360506,0.103635697392691,
13.3619643809855));
#16422=CARTESIAN_POINT('Ctrl Pts',(0.0795422385599767,0.315671517116894,
13.3778793489676));
#16423=CARTESIAN_POINT('Ctrl Pts',(-0.22264354123035,0.237497894948556,
13.3937943169495));
#16424=CARTESIAN_POINT('Ctrl Pts',(-0.320144713407304,-0.0590168274036149,
13.4097092849316));
#16425=CARTESIAN_POINT('Ctrl Pts',(-0.123323209650487,-0.301275347423447,
13.4256242529136));
#16426=CARTESIAN_POINT('Ctrl Pts',(0.186872322983632,-0.266558826242796,
13.4415392208956));
#16427=CARTESIAN_POINT('Ctrl Pts',(0.325272617550382,0.013214488303052,
13.4574541888776));
#16428=CARTESIAN_POINT('Ctrl Pts',(0.164628800197782,0.280841935096709,
13.4733691568596));
#16429=CARTESIAN_POINT('Ctrl Pts',(-0.14734817258063,0.290274589224139,
13.4892841248416));
#16430=CARTESIAN_POINT('Ctrl Pts',(-0.323896433207958,0.0328579157047686,
13.5051990928236));
#16431=CARTESIAN_POINT('Ctrl Pts',(-0.202603063457104,-0.254790346364651,
13.5211140608057));
#16432=CARTESIAN_POINT('Ctrl Pts',(0.104805414110265,-0.308150272288416,
13.5370290287877));
#16433=CARTESIAN_POINT('Ctrl Pts',(0.316163772954992,-0.0783189326698027,
13.5529439967697));
#16434=CARTESIAN_POINT('Ctrl Pts',(0.236235615786759,0.223719310281602,
13.5688589647517));
#16435=CARTESIAN_POINT('Ctrl Pts',(0.0391509082027412,0.287422334004927,
13.5794689434064));
#16436=CARTESIAN_POINT('Ctrl Pts',(-0.0509883685250158,0.27042677322694,
13.5847739327337));
#16437=CARTESIAN_POINT('Ctrl Pts',(-0.128892185405305,0.264462557919726,
12.8));
#16438=CARTESIAN_POINT('Ctrl Pts',(-0.217043456109746,0.221499916944292,
12.8053049893273));
#16439=CARTESIAN_POINT('Ctrl Pts',(-0.345398484536424,0.0410652795717879,
12.815914967982));
#16440=CARTESIAN_POINT('Ctrl Pts',(-0.22114650529359,-0.268979892602724,
12.831829935964));
#16441=CARTESIAN_POINT('Ctrl Pts',(0.106818910626803,-0.331166493061688,
12.847744903946));
#16442=CARTESIAN_POINT('Ctrl Pts',(0.336388835887821,-0.0891799169672639,
12.863659871928));
#16443=CARTESIAN_POINT('Ctrl Pts',(0.256796730875014,0.234928861325839,
12.8795748399101));
#16444=CARTESIAN_POINT('Ctrl Pts',(-0.0589241833804849,0.34299244583165,
12.8954898078921));
#16445=CARTESIAN_POINT('Ctrl Pts',(-0.320451751579676,0.13576133104918,
12.9114047758741));
#16446=CARTESIAN_POINT('Ctrl Pts',(-0.287385961817181,-0.196296031812836,
12.9273197438561));
#16447=CARTESIAN_POINT('Ctrl Pts',(0.00989033587804837,-0.347883154882157,
12.9432347118381));
#16448=CARTESIAN_POINT('Ctrl Pts',(0.298071545602751,-0.179651107103685,
12.9591496798201));
#16449=CARTESIAN_POINT('Ctrl Pts',(0.312224956762261,0.153743104957905,
12.9750646478021));
#16450=CARTESIAN_POINT('Ctrl Pts',(0.0393369692138751,0.345794316743414,
12.9909796157841));
#16451=CARTESIAN_POINT('Ctrl Pts',(-0.269714770986793,0.219943488100861,
13.0068945837661));
#16452=CARTESIAN_POINT('Ctrl Pts',(-0.330807144199375,-0.108110329426179,
13.0228095517481));
#16453=CARTESIAN_POINT('Ctrl Pts',(-0.0877752982397562,-0.336773927964842,
13.0387245197302));
#16454=CARTESIAN_POINT('Ctrl Pts',(0.235951834402727,-0.255827920514781,
13.0546394877122));
#16455=CARTESIAN_POINT('Ctrl Pts',(0.342759086246525,0.0603108822058324,
13.0705544556942));
#16456=CARTESIAN_POINT('Ctrl Pts',(0.134454283317385,0.321003483414848,
13.0864694236762));
#16457=CARTESIAN_POINT('Ctrl Pts',(-0.197459680920473,0.28658483303326,
13.1023843916582));
#16458=CARTESIAN_POINT('Ctrl Pts',(-0.347841116473733,-0.0113026440685232,
13.1182993596402));
#16459=CARTESIAN_POINT('Ctrl Pts',(-0.178438391737831,-0.298799150112829,
13.1342143276222));
#16460=CARTESIAN_POINT('Ctrl Pts',(0.15500983613138,-0.311597725655869,
13.1501292956042));
#16461=CARTESIAN_POINT('Ctrl Pts',(0.345951362720365,-0.0379321307497152,
13.1660442635862));
#16462=CARTESIAN_POINT('Ctrl Pts',(0.218846055516222,0.270605978993662,
13.1819592315683));
#16463=CARTESIAN_POINT('Ctrl Pts',(-0.109453126074549,0.330365260127584,
13.1978741995503));
#16464=CARTESIAN_POINT('Ctrl Pts',(-0.33712769986341,0.0864066309199375,
13.2137891675323));
#16465=CARTESIAN_POINT('Ctrl Pts',(-0.254867383880897,-0.236989047310205,
13.2297041355143));
#16466=CARTESIAN_POINT('Ctrl Pts',(0.0617026451075722,-0.342511277942956,
13.2456191034963));
#16467=CARTESIAN_POINT('Ctrl Pts',(0.321546980429126,-0.133149281376369,
13.2615340714783));
#16468=CARTESIAN_POINT('Ctrl Pts',(0.285780401073082,0.198622139841311,
13.2774490394603));
#16469=CARTESIAN_POINT('Ctrl Pts',(-0.0127154575823072,0.347792336391113,
13.2933640074423));
#16470=CARTESIAN_POINT('Ctrl Pts',(-0.299521487840284,0.177223217973269,
13.3092789754243));
#16471=CARTESIAN_POINT('Ctrl Pts',(-0.31096551941232,-0.156274244370674,
13.3251939434064));
#16472=CARTESIAN_POINT('Ctrl Pts',(-0.0365265803586308,-0.346102588837809,
13.3411089113884));
#16473=CARTESIAN_POINT('Ctrl Pts',(0.271492668970869,-0.217745062476789,
13.3570238793704));
#16474=CARTESIAN_POINT('Ctrl Pts',(0.329917974699552,0.110794133202663,
13.3729388473524));
#16475=CARTESIAN_POINT('Ctrl Pts',(0.0850364651946051,0.337475918005475,
13.3888538153344));
#16476=CARTESIAN_POINT('Ctrl Pts',(-0.238022214202109,0.253902603738722,
13.4047687833164));
#16477=CARTESIAN_POINT('Ctrl Pts',(-0.34225809169765,-0.0630933008708229,
13.4206837512984));
#16478=CARTESIAN_POINT('Ctrl Pts',(-0.131841522378367,-0.322085360670968,
13.4365987192804));
#16479=CARTESIAN_POINT('Ctrl Pts',(0.199780168083279,-0.284970862782778,
13.4525136872625));
#16480=CARTESIAN_POINT('Ctrl Pts',(0.347740195924013,0.0141272535823796,
13.4684286552444));
#16481=CARTESIAN_POINT('Ctrl Pts',(0.176000216884672,0.300240549818435,
13.4843436232265));
#16482=CARTESIAN_POINT('Ctrl Pts',(-0.157525963261562,0.310324746327379,
13.5002585912085));
#16483=CARTESIAN_POINT('Ctrl Pts',(-0.34626895430378,0.035127512825642,
13.5161735591905));
#16484=CARTESIAN_POINT('Ctrl Pts',(-0.216597479099101,-0.27238949786687,
13.5320885271725));
#16485=CARTESIAN_POINT('Ctrl Pts',(0.112044645845283,-0.329435157704335,
13.5480034951545));
#16486=CARTESIAN_POINT('Ctrl Pts',(0.338002175465677,-0.0837286618106999,
13.5639184631365));
#16487=CARTESIAN_POINT('Ctrl Pts',(0.252553135079664,0.239172289924649,
13.5798334311185));
#16488=CARTESIAN_POINT('Ctrl Pts',(0.0418551816367257,0.30727547708294,
13.5904434097732));
#16489=CARTESIAN_POINT('Ctrl Pts',(-0.0545102916878278,0.289105980740814,
13.5957483991005));
#16490=CARTESIAN_POINT('Ctrl Pts',(-0.294362671296069,-0.000253937998619662,
13.417782388291));
#16491=CARTESIAN_POINT('Ctrl Pts',(-0.294525507057634,-0.0181030578418672,
13.4187495092935));
#16492=CARTESIAN_POINT('Ctrl Pts',(-0.293042212129893,-0.035925170963799,
13.419716630296));
#16493=CARTESIAN_POINT('Ctrl Pts',(-0.289816017228513,-0.0534259934025893,
13.4206837512984));
#16494=CARTESIAN_POINT('Ctrl Pts',(-0.272119235257889,-0.149423987470871,
13.4259887406258));
#16495=CARTESIAN_POINT('Ctrl Pts',(-0.201980378818128,-0.235754674070919,
13.4312937299531));
#16496=CARTESIAN_POINT('Ctrl Pts',(-0.111640668854641,-0.272734267722911,
13.4365987192804));
#16497=CARTESIAN_POINT('Ctrl Pts',(-0.0213009588911521,-0.309713861374905,
13.4419037086078));
#16498=CARTESIAN_POINT('Ctrl Pts',(0.089239604596064,-0.297342362078841,
13.4472086979351));
#16499=CARTESIAN_POINT('Ctrl Pts',(0.169169890979795,-0.241306926369949,
13.4525136872624));
#16500=CARTESIAN_POINT('Ctrl Pts',(0.249100177363524,-0.185271490661058,
13.4578186765898));
#16501=CARTESIAN_POINT('Ctrl Pts',(0.298420186643769,-0.0855721185393391,
13.4631236659171));
#16502=CARTESIAN_POINT('Ctrl Pts',(0.294456861444001,0.011963116894196,
13.4684286552444));
#16503=CARTESIAN_POINT('Ctrl Pts',(0.290493536244233,0.109498352327731,
13.4737336445718));
#16504=CARTESIAN_POINT('Ctrl Pts',(0.233246876564453,0.204869451073082,
13.4790386338991));
#16505=CARTESIAN_POINT('Ctrl Pts',(0.149035850033524,0.254235699863916,
13.4843436232265));
#16506=CARTESIAN_POINT('Ctrl Pts',(0.0648248235025946,0.30360194865475,
13.4896486125538));
#16507=CARTESIAN_POINT('Ctrl Pts',(-0.0463505698794843,0.306963347491064,
13.4949536018811));
#16508=CARTESIAN_POINT('Ctrl Pts',(-0.133395431744227,0.262777841325598,
13.5002585912085));
#16509=CARTESIAN_POINT('Ctrl Pts',(-0.163703451423551,0.247392956316707,
13.5021057274723));
#16510=CARTESIAN_POINT('Ctrl Pts',(-0.191086000567156,0.226243711349668,
13.5039528637362));
#16511=CARTESIAN_POINT('Ctrl Pts',(-0.214321504642992,0.201109806014066,
13.5058));
#16512=CARTESIAN_POINT('Ctrl Pts',(-0.138011838534635,-0.19337538317794,
12.8));
#16513=CARTESIAN_POINT('Ctrl Pts',(-0.142822234716732,-0.190758128899072,
12.8));
#16514=CARTESIAN_POINT('Ctrl Pts',(-0.147526903047439,-0.187967753105685,
12.8));
#16515=CARTESIAN_POINT('Ctrl Pts',(-0.1521153417148,-0.185006306498425,
12.8));
#16516=CARTESIAN_POINT('Ctrl Pts',(-0.162156783890052,-0.178525410268204,
12.8));
#16517=CARTESIAN_POINT('Ctrl Pts',(-0.171642243951589,-0.17122677990977,
12.8));
#16518=CARTESIAN_POINT('Ctrl Pts',(-0.18054346266442,-0.163220362486912,
12.8));
#16519=CARTESIAN_POINT('Ctrl Pts',(-0.185992032158252,-0.158319514284835,
12.8));
#16520=CARTESIAN_POINT('Ctrl Pts',(-0.191225243452385,-0.153148297109027,
12.8));
#16521=CARTESIAN_POINT('Ctrl Pts',(-0.196212723907213,-0.147754132341615,
12.8));
#16522=CARTESIAN_POINT('Ctrl Pts',(-0.202978562151886,-0.140436600651622,
12.8));
#16523=CARTESIAN_POINT('Ctrl Pts',(-0.209300021277213,-0.132703531992446,
12.8));
#16524=CARTESIAN_POINT('Ctrl Pts',(-0.215160567422495,-0.124614033470671,
12.8));
#16525=CARTESIAN_POINT('Ctrl Pts',(-0.218668715917161,-0.119771624357552,
12.8));
#16526=CARTESIAN_POINT('Ctrl Pts',(-0.222011627016975,-0.114801320422425,
12.8));
#16527=CARTESIAN_POINT('Ctrl Pts',(-0.225184859023271,-0.109714472354803,
12.8));
#16528=CARTESIAN_POINT('Ctrl Pts',(-0.228211935744122,-0.104861918448424,
12.8));
#16529=CARTESIAN_POINT('Ctrl Pts',(-0.231085348796075,-0.0999011605270764,
12.8));
#16530=CARTESIAN_POINT('Ctrl Pts',(-0.233790550755382,-0.09486224802396,
12.8));
#16531=CARTESIAN_POINT('Ctrl Pts',(-0.241364933609335,-0.0807536331995264,
12.8));
#16532=CARTESIAN_POINT('Ctrl Pts',(-0.247644353527102,-0.0660037746918586,
12.8));
#16533=CARTESIAN_POINT('Ctrl Pts',(-0.252557798454291,-0.0508304825079511,
12.8));
#16534=CARTESIAN_POINT('Ctrl Pts',(-0.255926241889587,-0.0404283354998718,
12.8));
#16535=CARTESIAN_POINT('Ctrl Pts',(-0.258652125794692,-0.0298261112740156,
12.8));
#16536=CARTESIAN_POINT('Ctrl Pts',(-0.260701325119157,-0.0190856734862765,
12.8));
#16537=CARTESIAN_POINT('Ctrl Pts',(-0.26182904176174,-0.0131749891046926,
12.8));
#16538=CARTESIAN_POINT('Ctrl Pts',(-0.262751878512061,-0.00721720616864429,
12.8));
#16539=CARTESIAN_POINT('Ctrl Pts',(-0.26346009243944,-0.00125328645715371,
12.8));
#16540=CARTESIAN_POINT('Ctrl Pts',(-0.264745555031066,0.00957168519646787,
12.8));
#16541=CARTESIAN_POINT('Ctrl Pts',(-0.265328748128811,0.0204329089429716,
12.8));
#16542=CARTESIAN_POINT('Ctrl Pts',(-0.265185345887169,0.0312672356517,12.8));
#16543=CARTESIAN_POINT('Ctrl Pts',(-0.265031299079076,0.042905780685675,
12.8));
#16544=CARTESIAN_POINT('Ctrl Pts',(-0.264039219970955,0.0545135318648275,
12.8));
#16545=CARTESIAN_POINT('Ctrl Pts',(-0.262262766017228,0.066031106495167,
12.8));
#16546=CARTESIAN_POINT('Ctrl Pts',(-0.261137536932211,0.0733264883629122,
12.8));
#16547=CARTESIAN_POINT('Ctrl Pts',(-0.25969728945567,0.0805857612874066,
12.8));
#16548=CARTESIAN_POINT('Ctrl Pts',(-0.257952591865992,0.0877939534757336,
12.8));
#16549=CARTESIAN_POINT('Ctrl Pts',(-0.256901952665834,0.0921346537324037,
12.8));
#16550=CARTESIAN_POINT('Ctrl Pts',(-0.255740653864154,0.0964566832907016,
12.8));
#16551=CARTESIAN_POINT('Ctrl Pts',(-0.254475469588544,0.100742853504323,
12.8));
#16552=CARTESIAN_POINT('Ctrl Pts',(-0.249793608361451,0.116603984979587,
12.8));
#16553=CARTESIAN_POINT('Ctrl Pts',(-0.243682406310052,0.132021898855319,
12.8));
#16554=CARTESIAN_POINT('Ctrl Pts',(-0.23628872388492,0.146835744613901,
12.8));
#16555=CARTESIAN_POINT('Ctrl Pts',(-0.229571591801449,0.160294066584336,
12.8));
#16556=CARTESIAN_POINT('Ctrl Pts',(-0.221794948880427,0.173254712590635,
12.8));
#16557=CARTESIAN_POINT('Ctrl Pts',(-0.213034382217665,0.185591542266393,
12.8));
#16558=CARTESIAN_POINT('Ctrl Pts',(-0.210424335567796,0.189267069455986,
12.8));
#16559=CARTESIAN_POINT('Ctrl Pts',(-0.207727064739911,0.192886342584116,
12.8));
#16560=CARTESIAN_POINT('Ctrl Pts',(-0.204952945248888,0.196435599584694,
12.8));
#16561=CARTESIAN_POINT('Ctrl Pts',(-0.194195780011085,0.210198504949868,
12.8));
#16562=CARTESIAN_POINT('Ctrl Pts',(-0.182257287796659,0.222952674257295,
12.8));
#16563=CARTESIAN_POINT('Ctrl Pts',(-0.169272003354721,0.23451832610712,
12.8));
#16564=CARTESIAN_POINT('Ctrl Pts',(-0.156757744220975,0.245664448084392,
12.8));
#16565=CARTESIAN_POINT('Ctrl Pts',(-0.143270367034069,0.255707981058576,
12.8));
#16566=CARTESIAN_POINT('Ctrl Pts',(-0.128892185405305,0.264462557919726,
12.8));
#16567=CARTESIAN_POINT('Origin',(-3.51939854619125E-17,1.42943244214557E-17,
12.8));
#16568=CARTESIAN_POINT('Origin',(0.,0.,0.));
#16569=CARTESIAN_POINT('Origin',(-0.144337567297407,-0.25,-0.6));
#16570=CARTESIAN_POINT('',(-0.144337567297407,-0.25,-0.6));
#16571=CARTESIAN_POINT('',(0.144337567297406,-0.25,-0.6));
#16572=CARTESIAN_POINT('',(-0.0721687836487033,-0.25,-0.6));
#16573=CARTESIAN_POINT('',(-0.144337567297407,-0.25,-0.3));
#16574=CARTESIAN_POINT('',(-0.144337567297407,-0.25,-0.6));
#16575=CARTESIAN_POINT('',(0.144337567297406,-0.25,-0.3));
#16576=CARTESIAN_POINT('',(-0.144337567297407,-0.25,-0.3));
#16577=CARTESIAN_POINT('',(0.144337567297406,-0.25,-0.6));
#16578=CARTESIAN_POINT('Origin',(-0.288675134594813,3.53525079574969E-17,
-0.6));
#16579=CARTESIAN_POINT('',(-0.288675134594813,3.53525079574969E-17,-0.6));
#16580=CARTESIAN_POINT('',(-0.252590742770461,-0.0625,-0.6));
#16581=CARTESIAN_POINT('',(-0.288675134594813,5.55111512312578E-17,-0.3));
#16582=CARTESIAN_POINT('',(-0.288675134594813,3.53525079574969E-17,-0.6));
#16583=CARTESIAN_POINT('',(-0.288675134594813,3.53525079574969E-17,-0.3));
#16584=CARTESIAN_POINT('Origin',(-0.144337567297406,0.25,-0.6));
#16585=CARTESIAN_POINT('',(-0.144337567297406,0.25,-0.6));
#16586=CARTESIAN_POINT('',(-0.180421959121758,0.1875,-0.6));
#16587=CARTESIAN_POINT('',(-0.144337567297406,0.25,-0.3));
#16588=CARTESIAN_POINT('',(-0.144337567297406,0.25,-0.6));
#16589=CARTESIAN_POINT('',(-0.144337567297406,0.25,-0.3));
#16590=CARTESIAN_POINT('Origin',(0.144337567297406,0.25,-0.6));
#16591=CARTESIAN_POINT('',(0.144337567297406,0.25,-0.6));
#16592=CARTESIAN_POINT('',(0.0721687836487033,0.25,-0.6));
#16593=CARTESIAN_POINT('',(0.144337567297406,0.25,-0.3));
#16594=CARTESIAN_POINT('',(0.144337567297406,0.25,-0.6));
#16595=CARTESIAN_POINT('',(0.144337567297406,0.25,-0.3));
#16596=CARTESIAN_POINT('Origin',(0.288675134594813,0.,-0.6));
#16597=CARTESIAN_POINT('',(0.288675134594813,0.,-0.6));
#16598=CARTESIAN_POINT('',(0.252590742770461,0.0625,-0.6));
#16599=CARTESIAN_POINT('',(0.288675134594813,0.,-0.3));
#16600=CARTESIAN_POINT('',(0.288675134594813,0.,-0.6));
#16601=CARTESIAN_POINT('',(0.288675134594813,0.,-0.3));
#16602=CARTESIAN_POINT('Origin',(0.144337567297406,-0.25,-0.6));
#16603=CARTESIAN_POINT('',(0.180421959121758,-0.1875,-0.6));
#16604=CARTESIAN_POINT('',(0.144337567297406,-0.25,-0.3));
#16605=CARTESIAN_POINT('Origin',(0.,0.,-0.3));
#16606=CARTESIAN_POINT('Origin',(0.,0.,0.));
#16607=CARTESIAN_POINT('',(-0.5,-6.12323399573677E-17,0.));
#16608=CARTESIAN_POINT('Origin',(0.,0.,0.));
#16609=CARTESIAN_POINT('Origin',(0.,0.,-0.6));
#16610=CARTESIAN_POINT('',(-0.5,-6.12323399573677E-17,-0.6));
#16611=CARTESIAN_POINT('',(-0.5,-6.12323399573677E-17,-0.6));
#16612=CARTESIAN_POINT('Origin',(0.,0.,-0.6));
#16613=CARTESIAN_POINT('Origin',(0.,0.,-0.6));
#16614=CARTESIAN_POINT('Origin',(0.,0.,13.6));
#16615=CARTESIAN_POINT('',(0.,0.,0.));
#16616=CARTESIAN_POINT('',(0.,0.,0.));
#16617=CARTESIAN_POINT('',(0.,0.,0.));
#16618=CARTESIAN_POINT('',(0.,0.,2.8));
#16619=CARTESIAN_POINT('',(0.,0.,4.2));
#16620=CARTESIAN_POINT('',(0.,0.,4.2));
#16621=CARTESIAN_POINT('',(0.,0.,4.2));
#16622=CARTESIAN_POINT('',(0.,0.,3.8));
#16623=CARTESIAN_POINT('',(0.,0.,7.));
#16624=CARTESIAN_POINT('',(0.,0.,0.));
#16625=CARTESIAN_POINT('',(0.,0.,4.2));
#16626=CARTESIAN_POINT('',(0.,0.,8.));
#16627=CARTESIAN_POINT('',(0.,0.,8.4));
#16628=CARTESIAN_POINT('',(0.,0.,0.));
#16629=CARTESIAN_POINT('',(0.,0.,0.));
#16630=CARTESIAN_POINT('',(0.,0.,0.));
#16631=CARTESIAN_POINT('',(0.516690055055129,0.472261989797114,0.));
#16632=CARTESIAN_POINT('',(0.,0.,0.));
#16633=CARTESIAN_POINT('',(0.,0.,0.));
#16634=CARTESIAN_POINT('',(0.,0.,0.));
#16635=CARTESIAN_POINT('',(0.,0.,-0.8));
#16636=CARTESIAN_POINT('',(0.516690055055129,0.472261989797114,4.2));
#16637=CARTESIAN_POINT('',(0.,0.,11.8));
#16638=CARTESIAN_POINT('',(0.,0.,0.));
#16639=CARTESIAN_POINT('',(0.,0.,0.));
#16640=CARTESIAN_POINT('',(0.,0.,12.8));
#16641=CARTESIAN_POINT('',(0.,0.,13.));
#16642=CARTESIAN_POINT('',(7.4,0.,12.8));
#16643=CARTESIAN_POINT('',(0.,7.4,12.8));
#16644=CARTESIAN_POINT('',(-7.4,0.,12.8));
#16645=CARTESIAN_POINT('',(0.,-7.4,12.8));
#16646=UNCERTAINTY_MEASURE_WITH_UNIT(LENGTH_MEASURE(0.001),#16688,
'DISTANCE_ACCURACY_VALUE',
'Maximum model space distance between geometric entities at asserted c
onnectivities');
#16647=UNCERTAINTY_MEASURE_WITH_UNIT(LENGTH_MEASURE(0.001),#16688,
'DISTANCE_ACCURACY_VALUE',
'Maximum model space distance between geometric entities at asserted c
onnectivities');
#16648=UNCERTAINTY_MEASURE_WITH_UNIT(LENGTH_MEASURE(0.001),#16688,
'DISTANCE_ACCURACY_VALUE',
'Maximum model space distance between geometric entities at asserted c
onnectivities');
#16649=UNCERTAINTY_MEASURE_WITH_UNIT(LENGTH_MEASURE(0.001),#16688,
'DISTANCE_ACCURACY_VALUE',
'Maximum model space distance between geometric entities at asserted c
onnectivities');
#16650=UNCERTAINTY_MEASURE_WITH_UNIT(LENGTH_MEASURE(0.001),#16688,
'DISTANCE_ACCURACY_VALUE',
'Maximum model space distance between geometric entities at asserted c
onnectivities');
#16651=UNCERTAINTY_MEASURE_WITH_UNIT(LENGTH_MEASURE(0.001),#16688,
'DISTANCE_ACCURACY_VALUE',
'Maximum model space distance between geometric entities at asserted c
onnectivities');
#16652=UNCERTAINTY_MEASURE_WITH_UNIT(LENGTH_MEASURE(0.001),#16688,
'DISTANCE_ACCURACY_VALUE',
'Maximum model space distance between geometric entities at asserted c
onnectivities');
#16653=UNCERTAINTY_MEASURE_WITH_UNIT(LENGTH_MEASURE(0.001),#16688,
'DISTANCE_ACCURACY_VALUE',
'Maximum model space distance between geometric entities at asserted c
onnectivities');
#16654=UNCERTAINTY_MEASURE_WITH_UNIT(LENGTH_MEASURE(0.001),#16688,
'DISTANCE_ACCURACY_VALUE',
'Maximum model space distance between geometric entities at asserted c
onnectivities');
#16655=UNCERTAINTY_MEASURE_WITH_UNIT(LENGTH_MEASURE(0.001),#16688,
'DISTANCE_ACCURACY_VALUE',
'Maximum model space distance between geometric entities at asserted c
onnectivities');
#16656=UNCERTAINTY_MEASURE_WITH_UNIT(LENGTH_MEASURE(0.001),#16688,
'DISTANCE_ACCURACY_VALUE',
'Maximum model space distance between geometric entities at asserted c
onnectivities');
#16657=UNCERTAINTY_MEASURE_WITH_UNIT(LENGTH_MEASURE(0.001),#16688,
'DISTANCE_ACCURACY_VALUE',
'Maximum model space distance between geometric entities at asserted c
onnectivities');
#16658=UNCERTAINTY_MEASURE_WITH_UNIT(LENGTH_MEASURE(0.001),#16688,
'DISTANCE_ACCURACY_VALUE',
'Maximum model space distance between geometric entities at asserted c
onnectivities');
#16659=UNCERTAINTY_MEASURE_WITH_UNIT(LENGTH_MEASURE(0.001),#16688,
'DISTANCE_ACCURACY_VALUE',
'Maximum model space distance between geometric entities at asserted c
onnectivities');
#16660=UNCERTAINTY_MEASURE_WITH_UNIT(LENGTH_MEASURE(0.001),#16688,
'DISTANCE_ACCURACY_VALUE',
'Maximum model space distance between geometric entities at asserted c
onnectivities');
#16661=UNCERTAINTY_MEASURE_WITH_UNIT(LENGTH_MEASURE(0.001),#16688,
'DISTANCE_ACCURACY_VALUE',
'Maximum model space distance between geometric entities at asserted c
onnectivities');
#16662=UNCERTAINTY_MEASURE_WITH_UNIT(LENGTH_MEASURE(0.001),#16688,
'DISTANCE_ACCURACY_VALUE',
'Maximum model space distance between geometric entities at asserted c
onnectivities');
#16663=UNCERTAINTY_MEASURE_WITH_UNIT(LENGTH_MEASURE(0.001),#16688,
'DISTANCE_ACCURACY_VALUE',
'Maximum model space distance between geometric entities at asserted c
onnectivities');
#16664=UNCERTAINTY_MEASURE_WITH_UNIT(LENGTH_MEASURE(0.001),#16688,
'DISTANCE_ACCURACY_VALUE',
'Maximum model space distance between geometric entities at asserted c
onnectivities');
#16665=UNCERTAINTY_MEASURE_WITH_UNIT(LENGTH_MEASURE(0.001),#16688,
'DISTANCE_ACCURACY_VALUE',
'Maximum model space distance between geometric entities at asserted c
onnectivities');
#16666=UNCERTAINTY_MEASURE_WITH_UNIT(LENGTH_MEASURE(0.001),#16688,
'DISTANCE_ACCURACY_VALUE',
'Maximum model space distance between geometric entities at asserted c
onnectivities');
#16667=(
GEOMETRIC_REPRESENTATION_CONTEXT(3)
GLOBAL_UNCERTAINTY_ASSIGNED_CONTEXT((#16646))
GLOBAL_UNIT_ASSIGNED_CONTEXT((#16688,#16690,#16691))
REPRESENTATION_CONTEXT('','3D')
);
#16668=(
GEOMETRIC_REPRESENTATION_CONTEXT(3)
GLOBAL_UNCERTAINTY_ASSIGNED_CONTEXT((#16647))
GLOBAL_UNIT_ASSIGNED_CONTEXT((#16688,#16690,#16691))
REPRESENTATION_CONTEXT('','3D')
);
#16669=(
GEOMETRIC_REPRESENTATION_CONTEXT(3)
GLOBAL_UNCERTAINTY_ASSIGNED_CONTEXT((#16648))
GLOBAL_UNIT_ASSIGNED_CONTEXT((#16688,#16690,#16691))
REPRESENTATION_CONTEXT('','3D')
);
#16670=(
GEOMETRIC_REPRESENTATION_CONTEXT(3)
GLOBAL_UNCERTAINTY_ASSIGNED_CONTEXT((#16649))
GLOBAL_UNIT_ASSIGNED_CONTEXT((#16688,#16690,#16691))
REPRESENTATION_CONTEXT('','3D')
);
#16671=(
GEOMETRIC_REPRESENTATION_CONTEXT(3)
GLOBAL_UNCERTAINTY_ASSIGNED_CONTEXT((#16650))
GLOBAL_UNIT_ASSIGNED_CONTEXT((#16688,#16690,#16691))
REPRESENTATION_CONTEXT('','3D')
);
#16672=(
GEOMETRIC_REPRESENTATION_CONTEXT(3)
GLOBAL_UNCERTAINTY_ASSIGNED_CONTEXT((#16651))
GLOBAL_UNIT_ASSIGNED_CONTEXT((#16688,#16690,#16691))
REPRESENTATION_CONTEXT('','3D')
);
#16673=(
GEOMETRIC_REPRESENTATION_CONTEXT(3)
GLOBAL_UNCERTAINTY_ASSIGNED_CONTEXT((#16652))
GLOBAL_UNIT_ASSIGNED_CONTEXT((#16688,#16690,#16691))
REPRESENTATION_CONTEXT('','3D')
);
#16674=(
GEOMETRIC_REPRESENTATION_CONTEXT(3)
GLOBAL_UNCERTAINTY_ASSIGNED_CONTEXT((#16653))
GLOBAL_UNIT_ASSIGNED_CONTEXT((#16688,#16690,#16691))
REPRESENTATION_CONTEXT('','3D')
);
#16675=(
GEOMETRIC_REPRESENTATION_CONTEXT(3)
GLOBAL_UNCERTAINTY_ASSIGNED_CONTEXT((#16654))
GLOBAL_UNIT_ASSIGNED_CONTEXT((#16688,#16690,#16691))
REPRESENTATION_CONTEXT('','3D')
);
#16676=(
GEOMETRIC_REPRESENTATION_CONTEXT(3)
GLOBAL_UNCERTAINTY_ASSIGNED_CONTEXT((#16655))
GLOBAL_UNIT_ASSIGNED_CONTEXT((#16688,#16690,#16691))
REPRESENTATION_CONTEXT('','3D')
);
#16677=(
GEOMETRIC_REPRESENTATION_CONTEXT(3)
GLOBAL_UNCERTAINTY_ASSIGNED_CONTEXT((#16656))
GLOBAL_UNIT_ASSIGNED_CONTEXT((#16688,#16690,#16691))
REPRESENTATION_CONTEXT('','3D')
);
#16678=(
GEOMETRIC_REPRESENTATION_CONTEXT(3)
GLOBAL_UNCERTAINTY_ASSIGNED_CONTEXT((#16657))
GLOBAL_UNIT_ASSIGNED_CONTEXT((#16688,#16690,#16691))
REPRESENTATION_CONTEXT('','3D')
);
#16679=(
GEOMETRIC_REPRESENTATION_CONTEXT(3)
GLOBAL_UNCERTAINTY_ASSIGNED_CONTEXT((#16658))
GLOBAL_UNIT_ASSIGNED_CONTEXT((#16688,#16690,#16691))
REPRESENTATION_CONTEXT('','3D')
);
#16680=(
GEOMETRIC_REPRESENTATION_CONTEXT(3)
GLOBAL_UNCERTAINTY_ASSIGNED_CONTEXT((#16659))
GLOBAL_UNIT_ASSIGNED_CONTEXT((#16688,#16690,#16691))
REPRESENTATION_CONTEXT('','3D')
);
#16681=(
GEOMETRIC_REPRESENTATION_CONTEXT(3)
GLOBAL_UNCERTAINTY_ASSIGNED_CONTEXT((#16660))
GLOBAL_UNIT_ASSIGNED_CONTEXT((#16688,#16690,#16691))
REPRESENTATION_CONTEXT('','3D')
);
#16682=(
GEOMETRIC_REPRESENTATION_CONTEXT(3)
GLOBAL_UNCERTAINTY_ASSIGNED_CONTEXT((#16661))
GLOBAL_UNIT_ASSIGNED_CONTEXT((#16688,#16690,#16691))
REPRESENTATION_CONTEXT('','3D')
);
#16683=(
GEOMETRIC_REPRESENTATION_CONTEXT(3)
GLOBAL_UNCERTAINTY_ASSIGNED_CONTEXT((#16662))
GLOBAL_UNIT_ASSIGNED_CONTEXT((#16688,#16690,#16691))
REPRESENTATION_CONTEXT('','3D')
);
#16684=(
GEOMETRIC_REPRESENTATION_CONTEXT(3)
GLOBAL_UNCERTAINTY_ASSIGNED_CONTEXT((#16663))
GLOBAL_UNIT_ASSIGNED_CONTEXT((#16688,#16690,#16691))
REPRESENTATION_CONTEXT('','3D')
);
#16685=(
GEOMETRIC_REPRESENTATION_CONTEXT(3)
GLOBAL_UNCERTAINTY_ASSIGNED_CONTEXT((#16664))
GLOBAL_UNIT_ASSIGNED_CONTEXT((#16688,#16690,#16691))
REPRESENTATION_CONTEXT('','3D')
);
#16686=(
GEOMETRIC_REPRESENTATION_CONTEXT(3)
GLOBAL_UNCERTAINTY_ASSIGNED_CONTEXT((#16665))
GLOBAL_UNIT_ASSIGNED_CONTEXT((#16688,#16690,#16691))
REPRESENTATION_CONTEXT('','3D')
);
#16687=(
GEOMETRIC_REPRESENTATION_CONTEXT(3)
GLOBAL_UNCERTAINTY_ASSIGNED_CONTEXT((#16666))
GLOBAL_UNIT_ASSIGNED_CONTEXT((#16688,#16690,#16691))
REPRESENTATION_CONTEXT('','3D')
);
#16688=(
LENGTH_UNIT()
NAMED_UNIT(*)
SI_UNIT(.CENTI.,.METRE.)
);
#16689=(
LENGTH_UNIT()
NAMED_UNIT(*)
SI_UNIT($,.METRE.)
);
#16690=(
NAMED_UNIT(*)
PLANE_ANGLE_UNIT()
SI_UNIT($,.RADIAN.)
);
#16691=(
NAMED_UNIT(*)
SI_UNIT($,.STERADIAN.)
SOLID_ANGLE_UNIT()
);
#16692=SHAPE_DEFINITION_REPRESENTATION(#16712,#16763);
#16693=SHAPE_DEFINITION_REPRESENTATION(#16713,#16764);
#16694=SHAPE_DEFINITION_REPRESENTATION(#16714,#16765);
#16695=SHAPE_DEFINITION_REPRESENTATION(#16715,#16766);
#16696=SHAPE_DEFINITION_REPRESENTATION(#16716,#16767);
#16697=SHAPE_DEFINITION_REPRESENTATION(#16717,#16768);
#16698=SHAPE_DEFINITION_REPRESENTATION(#16718,#16769);
#16699=SHAPE_DEFINITION_REPRESENTATION(#16719,#16770);
#16700=SHAPE_DEFINITION_REPRESENTATION(#16720,#16771);
#16701=SHAPE_DEFINITION_REPRESENTATION(#16721,#16772);
#16702=SHAPE_DEFINITION_REPRESENTATION(#16722,#16773);
#16703=SHAPE_DEFINITION_REPRESENTATION(#16723,#16774);
#16704=SHAPE_DEFINITION_REPRESENTATION(#16724,#16775);
#16705=SHAPE_DEFINITION_REPRESENTATION(#16725,#16776);
#16706=SHAPE_DEFINITION_REPRESENTATION(#16726,#16777);
#16707=SHAPE_DEFINITION_REPRESENTATION(#16727,#16778);
#16708=SHAPE_DEFINITION_REPRESENTATION(#16728,#16779);
#16709=SHAPE_DEFINITION_REPRESENTATION(#16729,#16780);
#16710=SHAPE_DEFINITION_REPRESENTATION(#16730,#16781);
#16711=SHAPE_DEFINITION_REPRESENTATION(#16731,#16782);
#16712=PRODUCT_DEFINITION_SHAPE('',$,#16784);
#16713=PRODUCT_DEFINITION_SHAPE('',$,#16785);
#16714=PRODUCT_DEFINITION_SHAPE('',$,#16786);
#16715=PRODUCT_DEFINITION_SHAPE('',$,#16787);
#16716=PRODUCT_DEFINITION_SHAPE('',$,#16788);
#16717=PRODUCT_DEFINITION_SHAPE('',$,#16789);
#16718=PRODUCT_DEFINITION_SHAPE('',$,#16790);
#16719=PRODUCT_DEFINITION_SHAPE('',$,#16791);
#16720=PRODUCT_DEFINITION_SHAPE('',$,#16792);
#16721=PRODUCT_DEFINITION_SHAPE('',$,#16793);
#16722=PRODUCT_DEFINITION_SHAPE('',$,#16794);
#16723=PRODUCT_DEFINITION_SHAPE('',$,#16795);
#16724=PRODUCT_DEFINITION_SHAPE('',$,#16796);
#16725=PRODUCT_DEFINITION_SHAPE('',$,#16797);
#16726=PRODUCT_DEFINITION_SHAPE('',$,#16798);
#16727=PRODUCT_DEFINITION_SHAPE('',$,#16799);
#16728=PRODUCT_DEFINITION_SHAPE('',$,#16800);
#16729=PRODUCT_DEFINITION_SHAPE('',$,#16801);
#16730=PRODUCT_DEFINITION_SHAPE('',$,#16802);
#16731=PRODUCT_DEFINITION_SHAPE('',$,#16803);
#16732=PRODUCT_DEFINITION_SHAPE($,$,#104);
#16733=PRODUCT_DEFINITION_SHAPE($,$,#105);
#16734=PRODUCT_DEFINITION_SHAPE($,$,#106);
#16735=PRODUCT_DEFINITION_SHAPE($,$,#107);
#16736=PRODUCT_DEFINITION_SHAPE($,$,#108);
#16737=PRODUCT_DEFINITION_SHAPE($,$,#109);
#16738=PRODUCT_DEFINITION_SHAPE($,$,#110);
#16739=PRODUCT_DEFINITION_SHAPE($,$,#111);
#16740=PRODUCT_DEFINITION_SHAPE($,$,#112);
#16741=PRODUCT_DEFINITION_SHAPE($,$,#113);
#16742=PRODUCT_DEFINITION_SHAPE($,$,#114);
#16743=PRODUCT_DEFINITION_SHAPE($,$,#115);
#16744=PRODUCT_DEFINITION_SHAPE($,$,#116);
#16745=PRODUCT_DEFINITION_SHAPE($,$,#117);
#16746=PRODUCT_DEFINITION_SHAPE($,$,#118);
#16747=PRODUCT_DEFINITION_SHAPE($,$,#119);
#16748=PRODUCT_DEFINITION_SHAPE($,$,#120);
#16749=PRODUCT_DEFINITION_SHAPE($,$,#121);
#16750=PRODUCT_DEFINITION_SHAPE($,$,#122);
#16751=PRODUCT_DEFINITION_SHAPE($,$,#123);
#16752=PRODUCT_DEFINITION_SHAPE($,$,#124);
#16753=PRODUCT_DEFINITION_SHAPE($,$,#125);
#16754=PRODUCT_DEFINITION_SHAPE($,$,#126);
#16755=PRODUCT_DEFINITION_SHAPE($,$,#127);
#16756=PRODUCT_DEFINITION_SHAPE($,$,#128);
#16757=PRODUCT_DEFINITION_SHAPE($,$,#129);
#16758=PRODUCT_DEFINITION_SHAPE($,$,#130);
#16759=PRODUCT_DEFINITION_SHAPE($,$,#131);
#16760=PRODUCT_DEFINITION_SHAPE($,$,#132);
#16761=PRODUCT_DEFINITION_SHAPE($,$,#133);
#16762=PRODUCT_DEFINITION_SHAPE($,$,#134);
#16763=SHAPE_REPRESENTATION('',(#6341,#6957,#6958,#6959,#6960,#6961,#6962,
#6963,#6964,#6965,#6966,#6967,#6968,#6969,#6970,#6971,#6972,#6973,#6974,
#6975,#6976,#6977,#6978,#6979,#6980,#6981,#6982,#6983,#6984,#6985,#6986,
#6987),#16667);
#16764=SHAPE_REPRESENTATION('',(#6342),#16668);
#16765=SHAPE_REPRESENTATION('',(#6451),#16669);
#16766=SHAPE_REPRESENTATION('',(#6480),#16670);
#16767=SHAPE_REPRESENTATION('',(#6553),#16671);
#16768=SHAPE_REPRESENTATION('',(#6562),#16672);
#16769=SHAPE_REPRESENTATION('',(#6712),#16673);
#16770=SHAPE_REPRESENTATION('',(#6715),#16674);
#16771=SHAPE_REPRESENTATION('',(#6778),#16675);
#16772=SHAPE_REPRESENTATION('',(#6824),#16676);
#16773=SHAPE_REPRESENTATION('',(#6833),#16677);
#16774=SHAPE_REPRESENTATION('',(#6842),#16678);
#16775=SHAPE_REPRESENTATION('',(#6851),#16679);
#16776=SHAPE_REPRESENTATION('',(#6860),#16680);
#16777=SHAPE_REPRESENTATION('',(#6871),#16681);
#16778=SHAPE_REPRESENTATION('',(#6880),#16682);
#16779=SHAPE_REPRESENTATION('',(#6889),#16683);
#16780=SHAPE_REPRESENTATION('',(#6898),#16684);
#16781=SHAPE_REPRESENTATION('',(#6907),#16685);
#16782=SHAPE_REPRESENTATION('',(#6918),#16686);
#16783=PRODUCT_DEFINITION_CONTEXT('part definition',#16845,'design');
#16784=PRODUCT_DEFINITION('MAS-349','MAS-349',#16804,#16783);
#16785=PRODUCT_DEFINITION('Stage casing','Stage casing',#16805,#16783);
#16786=PRODUCT_DEFINITION('Stage diaphragm','Stage diaphragm',#16806,#16783);
#16787=PRODUCT_DEFINITION('Radial impeller','Radial impeller',#16807,#16783);
#16788=PRODUCT_DEFINITION('Stage wear ring','Stage wear ring',#16808,#16783);
#16789=PRODUCT_DEFINITION('Inlet head','Inlet head',#16809,#16783);
#16790=PRODUCT_DEFINITION('Seal ring','Seal ring',#16810,#16783);
#16791=PRODUCT_DEFINITION('Outlet head','Outlet head',#16811,#16783);
#16792=PRODUCT_DEFINITION('Shaft','Shaft',#16812,#16783);
#16793=PRODUCT_DEFINITION('Lower spacer','Lower spacer',#16813,#16783);
#16794=PRODUCT_DEFINITION('Intermediate spacer','Intermediate spacer',#16814,
#16783);
#16795=PRODUCT_DEFINITION('Upper spacer','Upper spacer',#16815,#16783);
#16796=PRODUCT_DEFINITION('Inlet journal bushing',
'Inlet journal bushing',#16816,#16783);
#16797=PRODUCT_DEFINITION('Drive key','Drive key',#16817,#16783);
#16798=PRODUCT_DEFINITION('Outlet journal bushing',
'Outlet journal bushing',#16818,#16783);
#16799=PRODUCT_DEFINITION('Rotating seal ring','Rotating seal ring',#16819,
#16783);
#16800=PRODUCT_DEFINITION('Stationary seal ring','Stationary seal ring',
#16820,#16783);
#16801=PRODUCT_DEFINITION('Shaft thrust washer','Shaft thrust washer',#16821,
#16783);
#16802=PRODUCT_DEFINITION('Shaft retaining ring','Shaft retaining ring',
#16822,#16783);
#16803=PRODUCT_DEFINITION('Socket head tie bolt M6x136',
'Socket head tie bolt M6x136',#16823,#16783);
#16804=PRODUCT_DEFINITION_FORMATION('',$,#16847);
#16805=PRODUCT_DEFINITION_FORMATION('',$,#16848);
#16806=PRODUCT_DEFINITION_FORMATION('',$,#16849);
#16807=PRODUCT_DEFINITION_FORMATION('',$,#16850);
#16808=PRODUCT_DEFINITION_FORMATION('',$,#16851);
#16809=PRODUCT_DEFINITION_FORMATION('',$,#16852);
#16810=PRODUCT_DEFINITION_FORMATION('',$,#16853);
#16811=PRODUCT_DEFINITION_FORMATION('',$,#16854);
#16812=PRODUCT_DEFINITION_FORMATION('',$,#16855);
#16813=PRODUCT_DEFINITION_FORMATION('',$,#16856);
#16814=PRODUCT_DEFINITION_FORMATION('',$,#16857);
#16815=PRODUCT_DEFINITION_FORMATION('',$,#16858);
#16816=PRODUCT_DEFINITION_FORMATION('',$,#16859);
#16817=PRODUCT_DEFINITION_FORMATION('',$,#16860);
#16818=PRODUCT_DEFINITION_FORMATION('',$,#16861);
#16819=PRODUCT_DEFINITION_FORMATION('',$,#16862);
#16820=PRODUCT_DEFINITION_FORMATION('',$,#16863);
#16821=PRODUCT_DEFINITION_FORMATION('',$,#16864);
#16822=PRODUCT_DEFINITION_FORMATION('',$,#16865);
#16823=PRODUCT_DEFINITION_FORMATION('',$,#16866);
#16824=PRODUCT_RELATED_PRODUCT_CATEGORY('MAS-349','MAS-349',(#16847));
#16825=PRODUCT_RELATED_PRODUCT_CATEGORY('Stage casing','Stage casing',(#16848));
#16826=PRODUCT_RELATED_PRODUCT_CATEGORY('Stage diaphragm',
'Stage diaphragm',(#16849));
#16827=PRODUCT_RELATED_PRODUCT_CATEGORY('Radial impeller',
'Radial impeller',(#16850));
#16828=PRODUCT_RELATED_PRODUCT_CATEGORY('Stage wear ring',
'Stage wear ring',(#16851));
#16829=PRODUCT_RELATED_PRODUCT_CATEGORY('Inlet head','Inlet head',(#16852));
#16830=PRODUCT_RELATED_PRODUCT_CATEGORY('Seal ring','Seal ring',(#16853));
#16831=PRODUCT_RELATED_PRODUCT_CATEGORY('Outlet head','Outlet head',(#16854));
#16832=PRODUCT_RELATED_PRODUCT_CATEGORY('Shaft','Shaft',(#16855));
#16833=PRODUCT_RELATED_PRODUCT_CATEGORY('Lower spacer','Lower spacer',(#16856));
#16834=PRODUCT_RELATED_PRODUCT_CATEGORY('Intermediate spacer',
'Intermediate spacer',(#16857));
#16835=PRODUCT_RELATED_PRODUCT_CATEGORY('Upper spacer','Upper spacer',(#16858));
#16836=PRODUCT_RELATED_PRODUCT_CATEGORY('Inlet journal bushing',
'Inlet journal bushing',(#16859));
#16837=PRODUCT_RELATED_PRODUCT_CATEGORY('Drive key','Drive key',(#16860));
#16838=PRODUCT_RELATED_PRODUCT_CATEGORY('Outlet journal bushing',
'Outlet journal bushing',(#16861));
#16839=PRODUCT_RELATED_PRODUCT_CATEGORY('Rotating seal ring',
'Rotating seal ring',(#16862));
#16840=PRODUCT_RELATED_PRODUCT_CATEGORY('Stationary seal ring',
'Stationary seal ring',(#16863));
#16841=PRODUCT_RELATED_PRODUCT_CATEGORY('Shaft thrust washer',
'Shaft thrust washer',(#16864));
#16842=PRODUCT_RELATED_PRODUCT_CATEGORY('Shaft retaining ring',
'Shaft retaining ring',(#16865));
#16843=PRODUCT_RELATED_PRODUCT_CATEGORY('Socket head tie bolt M6x136',
'Socket head tie bolt M6x136',(#16866));
#16844=APPLICATION_PROTOCOL_DEFINITION('international standard',
'automotive_design',2009,#16845);
#16845=APPLICATION_CONTEXT(
'Core Data for Automotive Mechanical Design Process');
#16846=PRODUCT_CONTEXT('part definition',#16845,'mechanical');
#16847=PRODUCT('MAS-349','MAS-349',
'Independent two-stage semi-open centrifugal-pump CAD. Shared impeller
s, open-machinable return casings, removable diaphragms, bronze wear/j
ournal rings, volume-preserving seal instances, retained keyed shaft, 
opposed mechanical face rings and partly threaded tie hardware. Native
 shaft rotation. Geometric topology/clearance only; flow/head/efficien
cy, pressure, cavitation, balance, preload, face loading and secondary
 seal fits/bonds, material/thermal/tolerance selection and life unassi
gned. External drive, coupling, anchors and piping bolts omitted.',(#16846));
#16848=PRODUCT('Stage casing','Stage casing',$,(#16846));
#16849=PRODUCT('Stage diaphragm','Stage diaphragm',$,(#16846));
#16850=PRODUCT('Radial impeller','Radial impeller',$,(#16846));
#16851=PRODUCT('Stage wear ring','Stage wear ring',$,(#16846));
#16852=PRODUCT('Inlet head','Inlet head',$,(#16846));
#16853=PRODUCT('Seal ring','Seal ring',
'Reusable132mm mean-diameter ring,3mm circular free wire,2mm installed
 axial height and derived4.5mm radial width preserving cross-section a
rea. Native constrained ellipse and revolve; gland/material/pressure s
election unassigned.',(#16846));
#16854=PRODUCT('Outlet head','Outlet head',$,(#16846));
#16855=PRODUCT('Shaft','Shaft','Shaft',(#16846));
#16856=PRODUCT('Lower spacer','Lower spacer',$,(#16846));
#16857=PRODUCT('Intermediate spacer','Intermediate spacer',$,(#16846));
#16858=PRODUCT('Upper spacer','Upper spacer',$,(#16846));
#16859=PRODUCT('Inlet journal bushing','Inlet journal bushing',$,(#16846));
#16860=PRODUCT('Drive key','Drive key',$,(#16846));
#16861=PRODUCT('Outlet journal bushing','Outlet journal bushing',$,(#16846));
#16862=PRODUCT('Rotating seal ring','Rotating seal ring',$,(#16846));
#16863=PRODUCT('Stationary seal ring','Stationary seal ring',$,(#16846));
#16864=PRODUCT('Shaft thrust washer','Shaft thrust washer',$,(#16846));
#16865=PRODUCT('Shaft retaining ring','Shaft retaining ring',$,(#16846));
#16866=PRODUCT('Socket head tie bolt M6x136',
'Socket head tie bolt M6x136',$,(#16846));
#16867=PRESENTATION_STYLE_ASSIGNMENT((#16882));
#16868=PRESENTATION_STYLE_ASSIGNMENT((#16883));
#16869=PRESENTATION_STYLE_ASSIGNMENT((#16884));
#16870=PRESENTATION_STYLE_ASSIGNMENT((#16885));
#16871=PRESENTATION_STYLE_ASSIGNMENT((#16886));
#16872=PRESENTATION_STYLE_ASSIGNMENT((#16887));
#16873=PRESENTATION_STYLE_ASSIGNMENT((#16888));
#16874=PRESENTATION_STYLE_ASSIGNMENT((#16889));
#16875=PRESENTATION_STYLE_ASSIGNMENT((#16890));
#16876=PRESENTATION_STYLE_ASSIGNMENT((#16891));
#16877=PRESENTATION_STYLE_ASSIGNMENT((#16892));
#16878=PRESENTATION_STYLE_ASSIGNMENT((#16893));
#16879=PRESENTATION_STYLE_ASSIGNMENT((#16894));
#16880=PRESENTATION_STYLE_ASSIGNMENT((#16895));
#16881=PRESENTATION_STYLE_ASSIGNMENT((#16896));
#16882=SURFACE_STYLE_USAGE(.BOTH.,#16897);
#16883=SURFACE_STYLE_USAGE(.BOTH.,#16898);
#16884=SURFACE_STYLE_USAGE(.BOTH.,#16899);
#16885=SURFACE_STYLE_USAGE(.BOTH.,#16900);
#16886=SURFACE_STYLE_USAGE(.BOTH.,#16901);
#16887=SURFACE_STYLE_USAGE(.BOTH.,#16902);
#16888=SURFACE_STYLE_USAGE(.BOTH.,#16903);
#16889=SURFACE_STYLE_USAGE(.BOTH.,#16904);
#16890=SURFACE_STYLE_USAGE(.BOTH.,#16905);
#16891=SURFACE_STYLE_USAGE(.BOTH.,#16906);
#16892=SURFACE_STYLE_USAGE(.BOTH.,#16907);
#16893=SURFACE_STYLE_USAGE(.BOTH.,#16908);
#16894=SURFACE_STYLE_USAGE(.BOTH.,#16909);
#16895=SURFACE_STYLE_USAGE(.BOTH.,#16910);
#16896=SURFACE_STYLE_USAGE(.BOTH.,#16911);
#16897=SURFACE_SIDE_STYLE('',(#16912));
#16898=SURFACE_SIDE_STYLE('',(#16913));
#16899=SURFACE_SIDE_STYLE('',(#16914));
#16900=SURFACE_SIDE_STYLE('',(#16915));
#16901=SURFACE_SIDE_STYLE('',(#16916));
#16902=SURFACE_SIDE_STYLE('',(#16917));
#16903=SURFACE_SIDE_STYLE('',(#16918));
#16904=SURFACE_SIDE_STYLE('',(#16919));
#16905=SURFACE_SIDE_STYLE('',(#16920));
#16906=SURFACE_SIDE_STYLE('',(#16921));
#16907=SURFACE_SIDE_STYLE('',(#16922));
#16908=SURFACE_SIDE_STYLE('',(#16923));
#16909=SURFACE_SIDE_STYLE('',(#16924));
#16910=SURFACE_SIDE_STYLE('',(#16925));
#16911=SURFACE_SIDE_STYLE('',(#16926));
#16912=SURFACE_STYLE_FILL_AREA(#16927);
#16913=SURFACE_STYLE_FILL_AREA(#16928);
#16914=SURFACE_STYLE_FILL_AREA(#16929);
#16915=SURFACE_STYLE_FILL_AREA(#16930);
#16916=SURFACE_STYLE_FILL_AREA(#16931);
#16917=SURFACE_STYLE_FILL_AREA(#16932);
#16918=SURFACE_STYLE_FILL_AREA(#16933);
#16919=SURFACE_STYLE_FILL_AREA(#16934);
#16920=SURFACE_STYLE_FILL_AREA(#16935);
#16921=SURFACE_STYLE_FILL_AREA(#16936);
#16922=SURFACE_STYLE_FILL_AREA(#16937);
#16923=SURFACE_STYLE_FILL_AREA(#16938);
#16924=SURFACE_STYLE_FILL_AREA(#16939);
#16925=SURFACE_STYLE_FILL_AREA(#16940);
#16926=SURFACE_STYLE_FILL_AREA(#16941);
#16927=FILL_AREA_STYLE('Steel - Satin',(#16942));
#16928=FILL_AREA_STYLE('Dark blue',(#16943));
#16929=FILL_AREA_STYLE('Sky blue',(#16944));
#16930=FILL_AREA_STYLE('Light blue',(#16945));
#16931=FILL_AREA_STYLE('Wear ring gray',(#16946));
#16932=FILL_AREA_STYLE('Seal charcoal',(#16947));
#16933=FILL_AREA_STYLE('Shaft gray',(#16948));
#16934=FILL_AREA_STYLE('Spacer gray',(#16949));
#16935=FILL_AREA_STYLE('Journal gray',(#16950));
#16936=FILL_AREA_STYLE('Key gray',(#16951));
#16937=FILL_AREA_STYLE('Face seal light gray',(#16952));
#16938=FILL_AREA_STYLE('Face seal charcoal',(#16953));
#16939=FILL_AREA_STYLE('Washer gray',(#16954));
#16940=FILL_AREA_STYLE('Dark gray',(#16955));
#16941=FILL_AREA_STYLE('Tie bolt gray',(#16956));
#16942=FILL_AREA_STYLE_COLOUR('Steel - Satin',#16957);
#16943=FILL_AREA_STYLE_COLOUR('Dark blue',#16958);
#16944=FILL_AREA_STYLE_COLOUR('Sky blue',#16959);
#16945=FILL_AREA_STYLE_COLOUR('Light blue',#16960);
#16946=FILL_AREA_STYLE_COLOUR('Wear ring gray',#16961);
#16947=FILL_AREA_STYLE_COLOUR('Seal charcoal',#16962);
#16948=FILL_AREA_STYLE_COLOUR('Shaft gray',#16963);
#16949=FILL_AREA_STYLE_COLOUR('Spacer gray',#16964);
#16950=FILL_AREA_STYLE_COLOUR('Journal gray',#16965);
#16951=FILL_AREA_STYLE_COLOUR('Key gray',#16966);
#16952=FILL_AREA_STYLE_COLOUR('Face seal light gray',#16967);
#16953=FILL_AREA_STYLE_COLOUR('Face seal charcoal',#16968);
#16954=FILL_AREA_STYLE_COLOUR('Washer gray',#16969);
#16955=FILL_AREA_STYLE_COLOUR('Dark gray',#16970);
#16956=FILL_AREA_STYLE_COLOUR('Tie bolt gray',#16971);
#16957=COLOUR_RGB('Steel - Satin',0.627450980392157,0.627450980392157,0.627450980392157);
#16958=COLOUR_RGB('Dark blue',0.0901960784313725,0.270588235294118,0.513725490196078);
#16959=COLOUR_RGB('Sky blue',0.317647058823529,0.686274509803922,0.890196078431372);
#16960=COLOUR_RGB('Light blue',0.662745098039216,0.831372549019608,0.949019607843137);
#16961=COLOUR_RGB('Wear ring gray',0.725490196078431,0.752941176470588,
0.792156862745098);
#16962=COLOUR_RGB('Seal charcoal',0.164705882352941,0.184313725490196,0.211764705882353);
#16963=COLOUR_RGB('Shaft gray',0.576470588235294,0.615686274509804,0.666666666666667);
#16964=COLOUR_RGB('Spacer gray',0.576470588235294,0.615686274509804,0.666666666666667);
#16965=COLOUR_RGB('Journal gray',0.725490196078431,0.752941176470588,0.792156862745098);
#16966=COLOUR_RGB('Key gray',0.725490196078431,0.752941176470588,0.792156862745098);
#16967=COLOUR_RGB('Face seal light gray',0.725490196078431,0.752941176470588,
0.792156862745098);
#16968=COLOUR_RGB('Face seal charcoal',0.164705882352941,0.184313725490196,
0.211764705882353);
#16969=COLOUR_RGB('Washer gray',0.725490196078431,0.752941176470588,0.792156862745098);
#16970=COLOUR_RGB('Dark gray',0.250980392156863,0.282352941176471,0.32156862745098);
#16971=COLOUR_RGB('Tie bolt gray',0.407843137254902,0.447058823529412,0.498039215686275);
ENDSEC;
END-ISO-10303-21;
